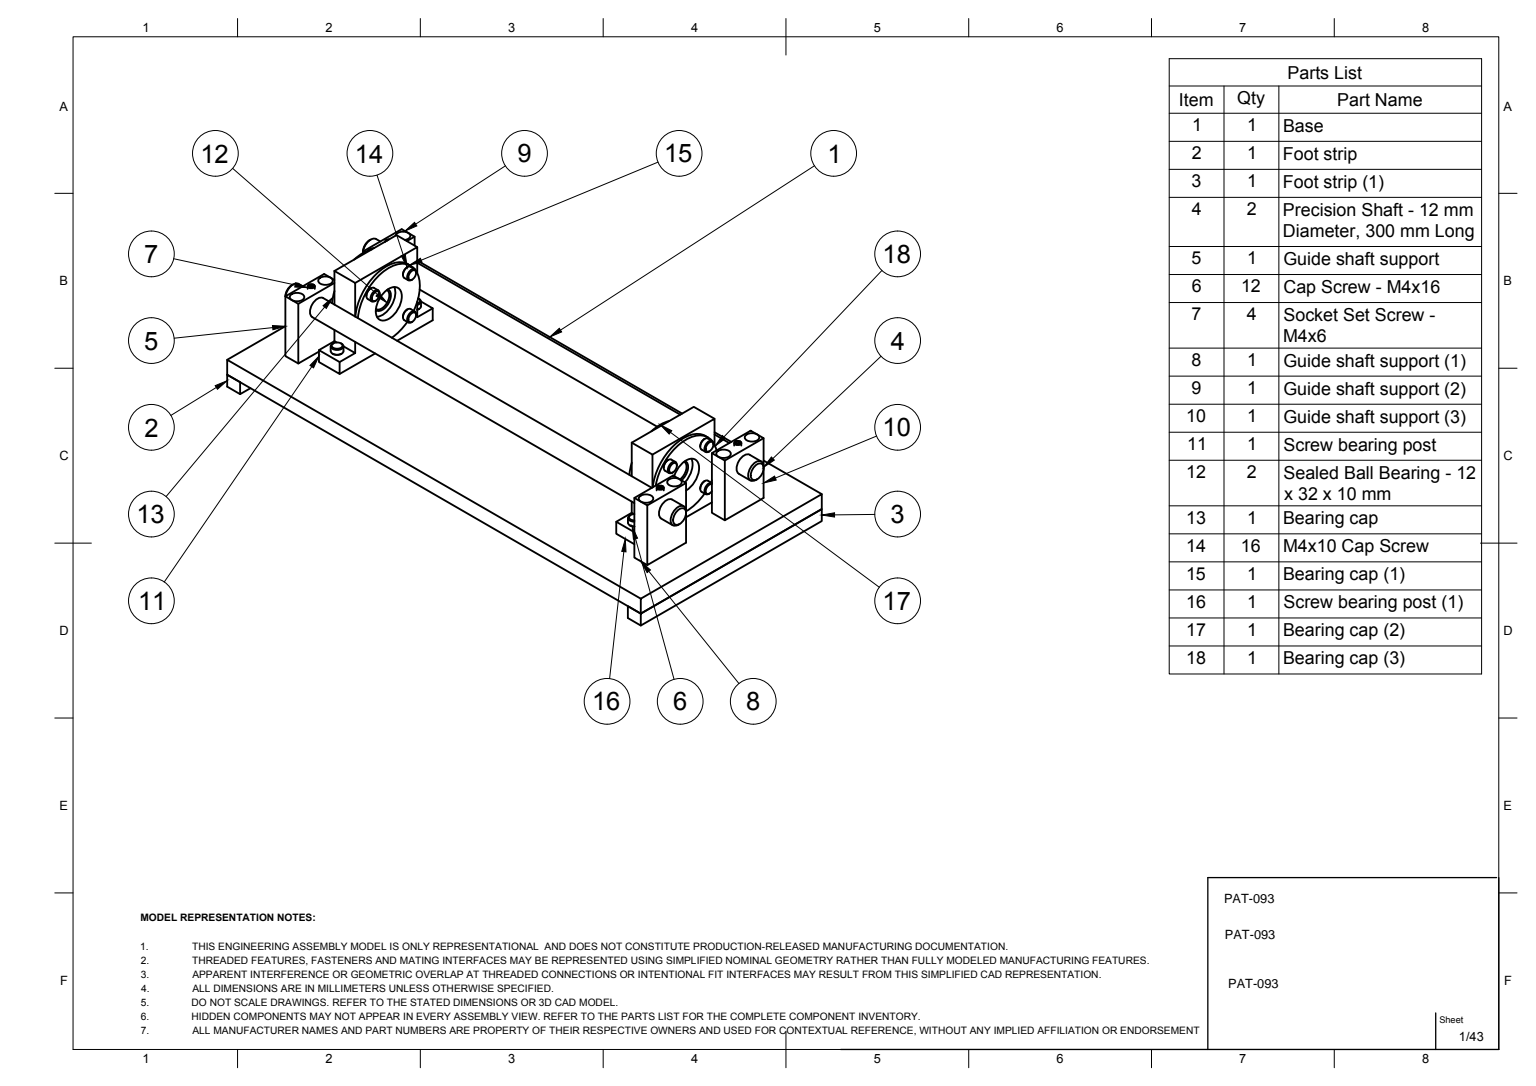
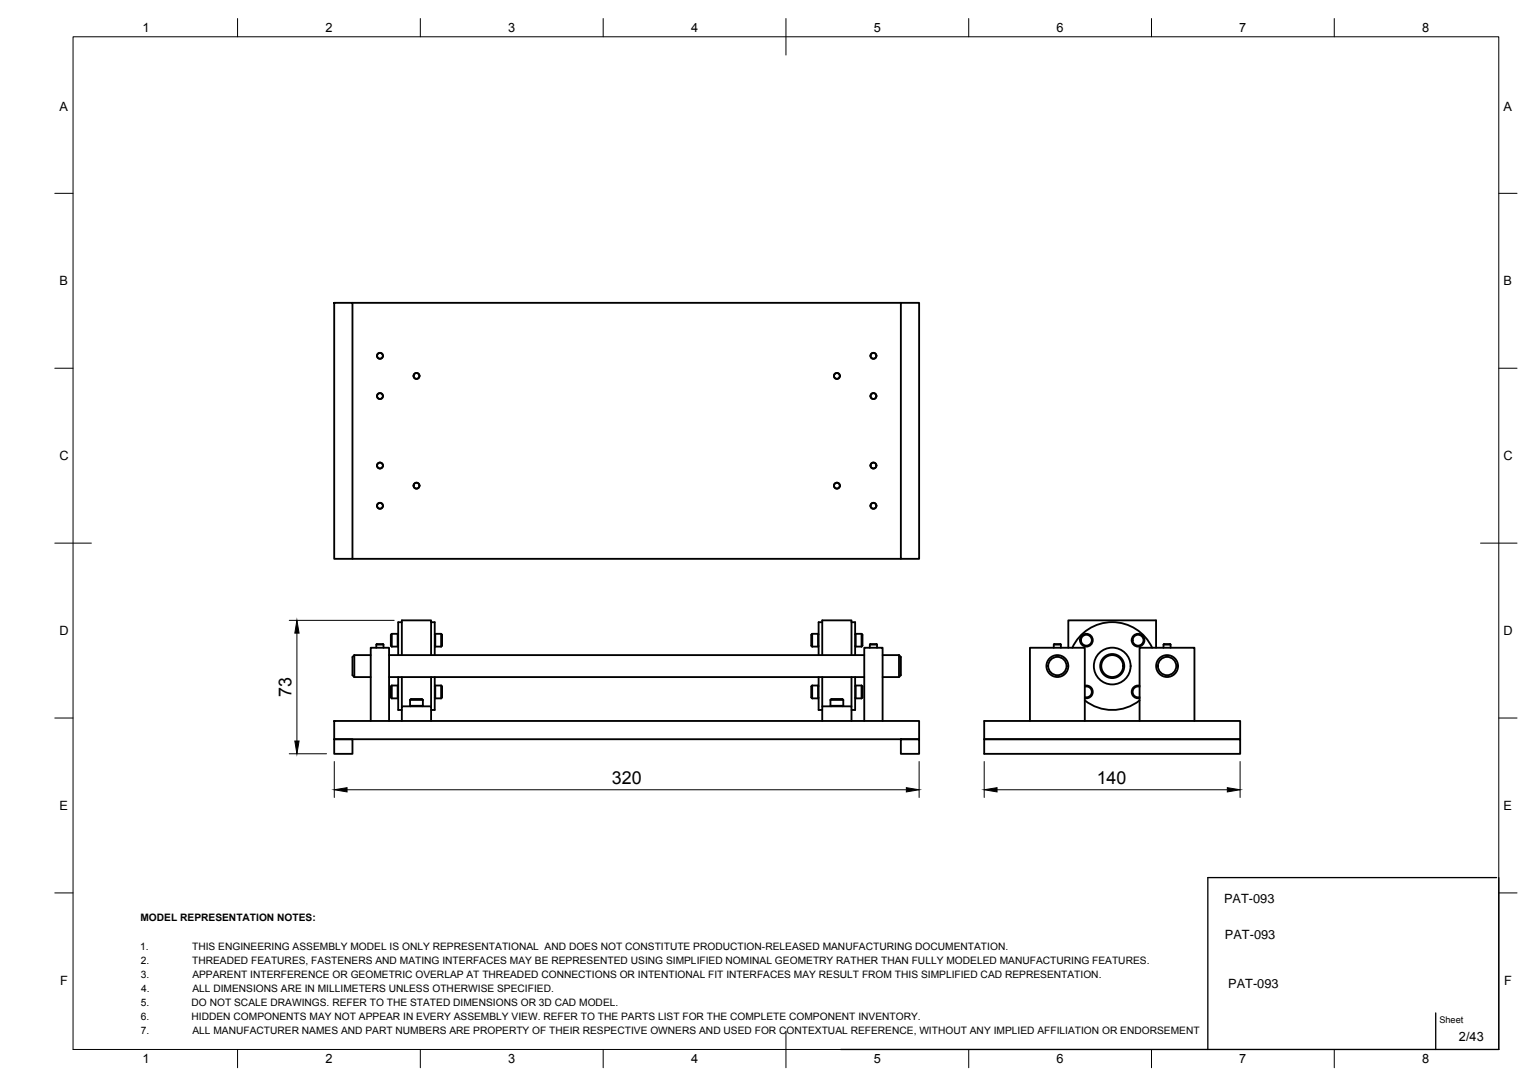
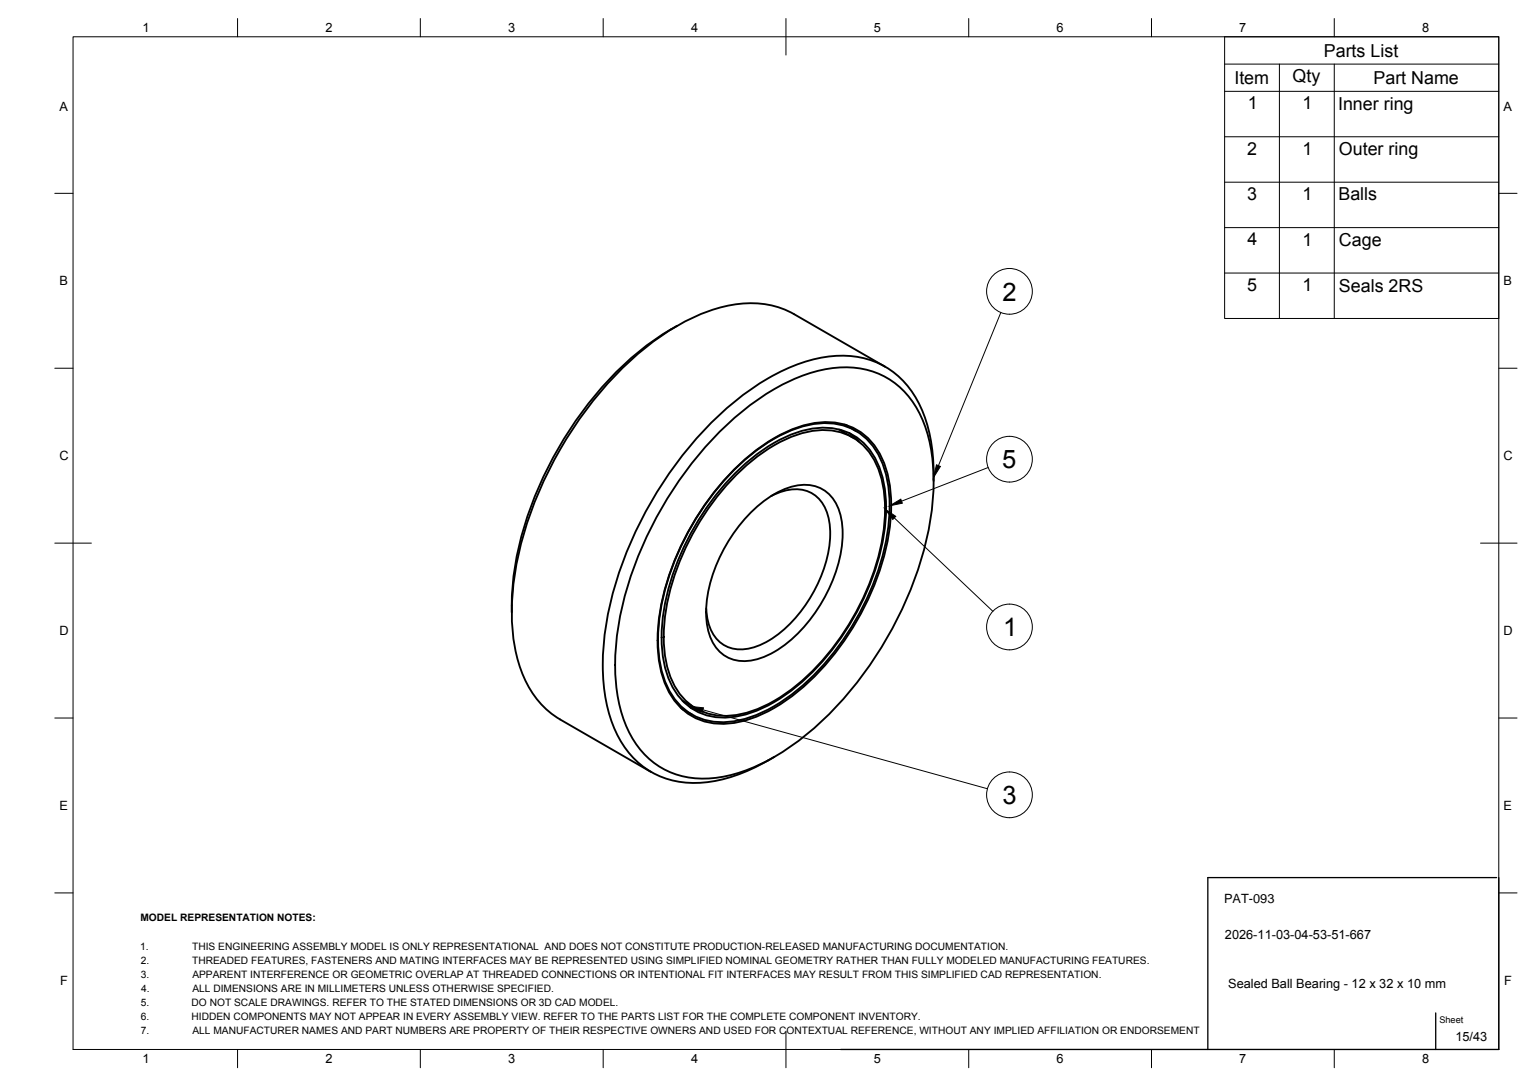
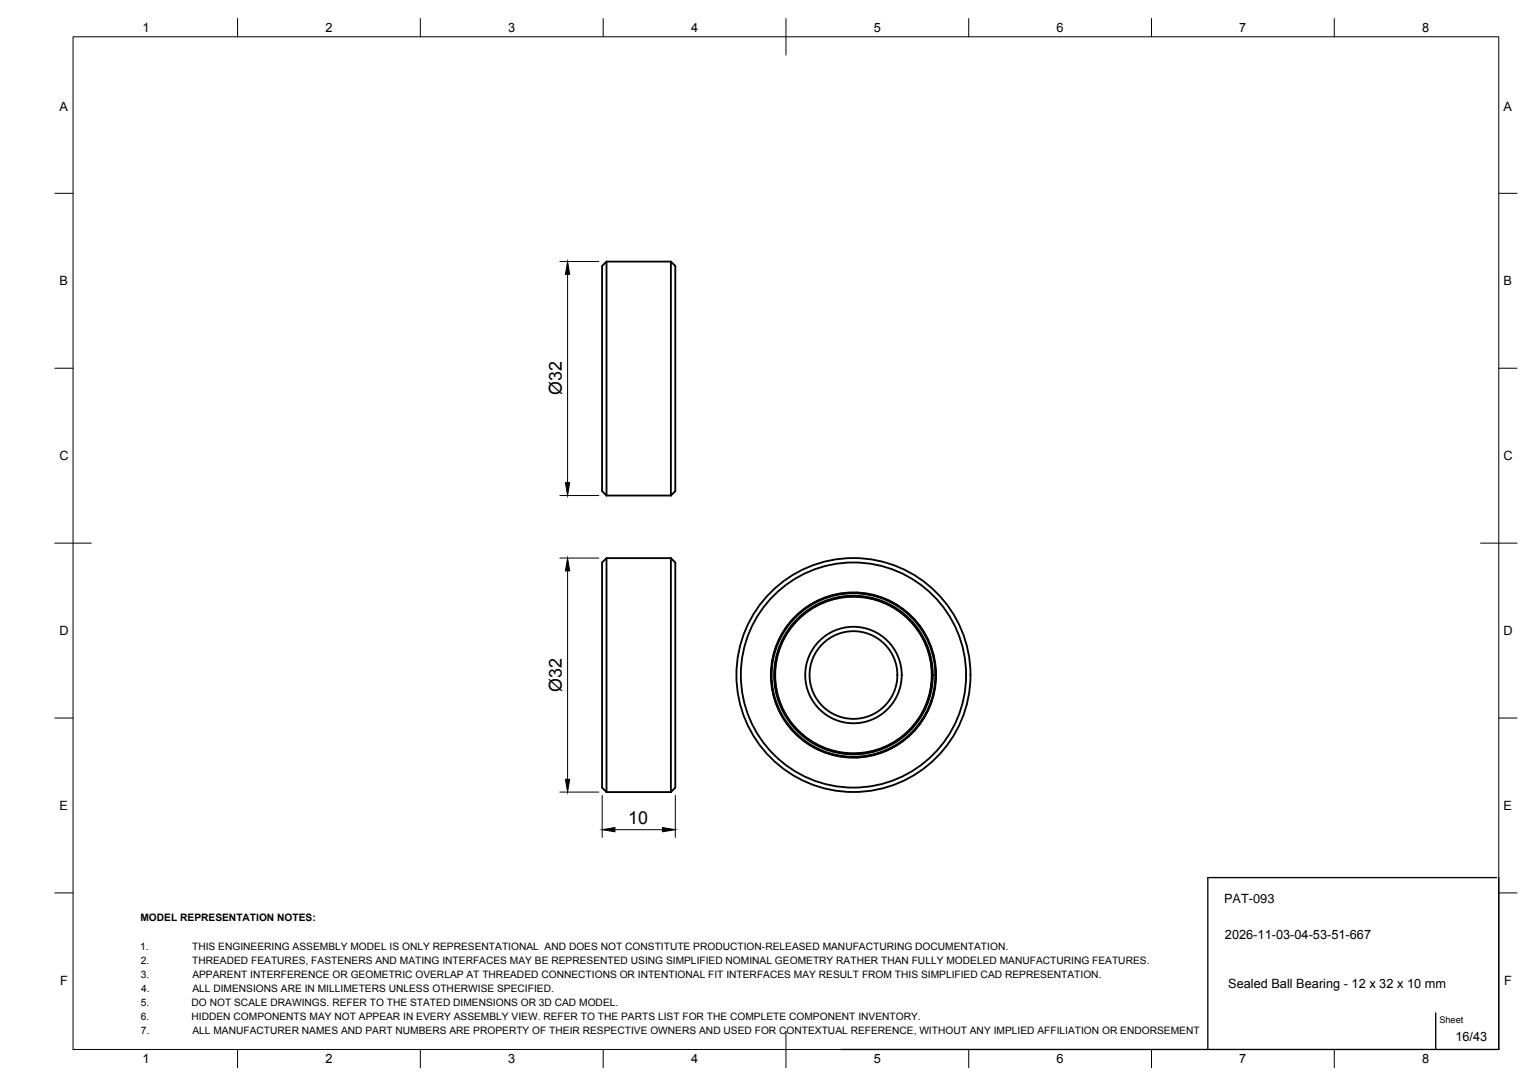
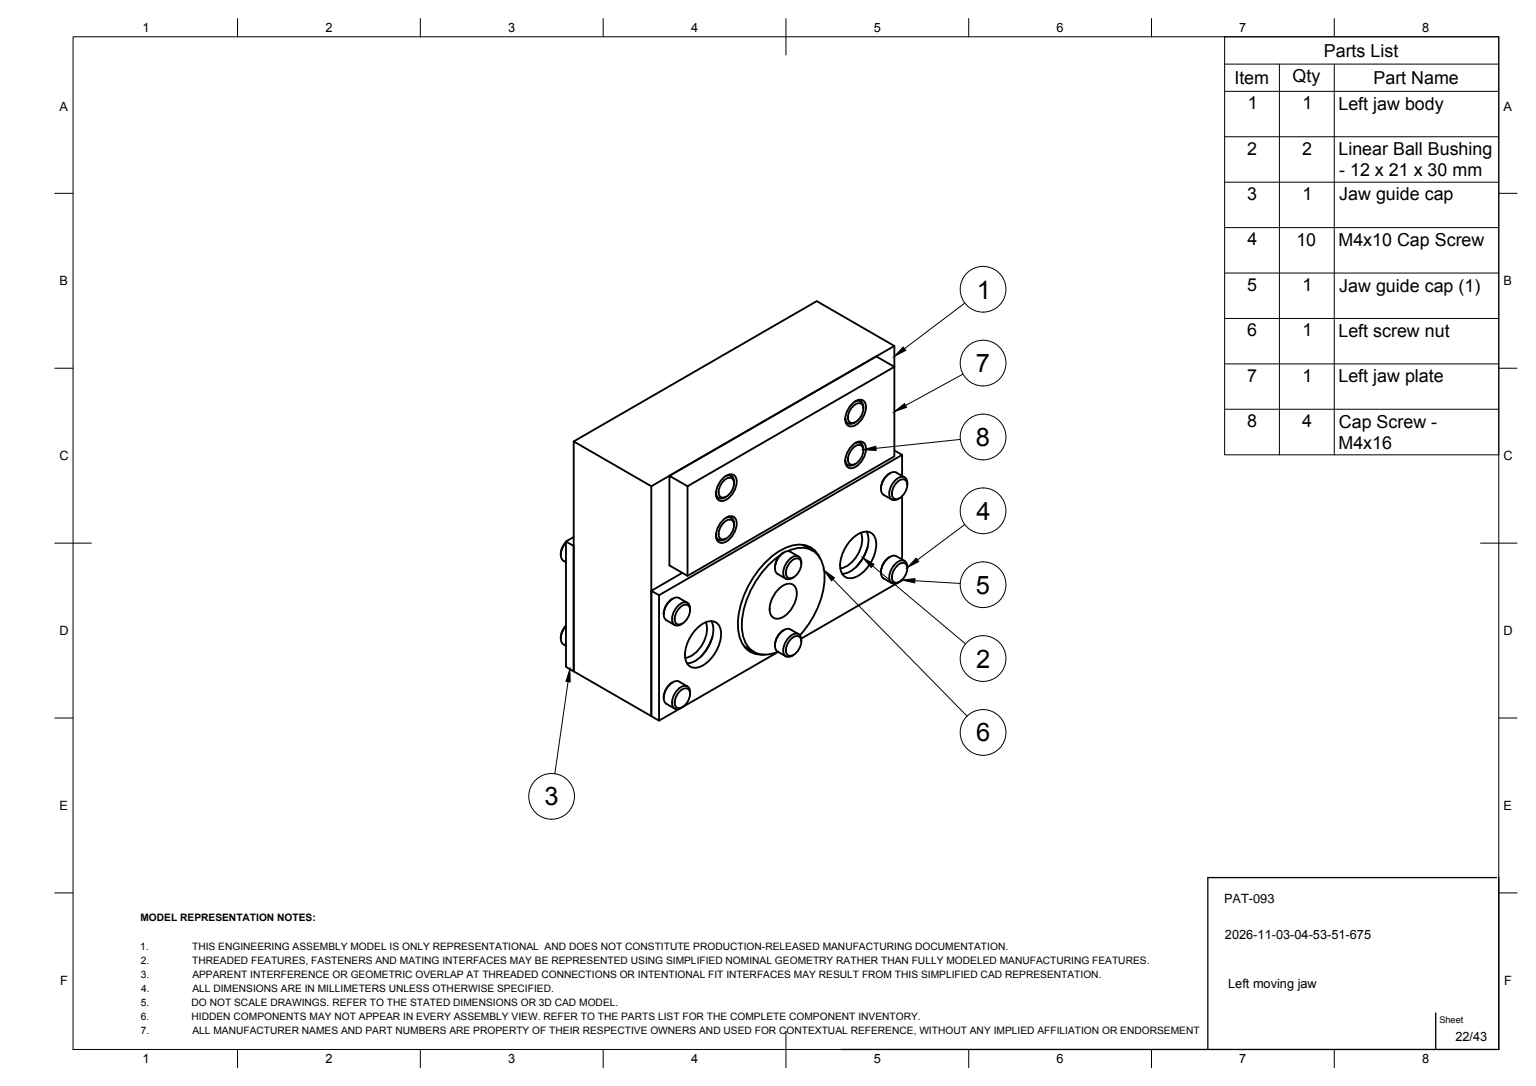
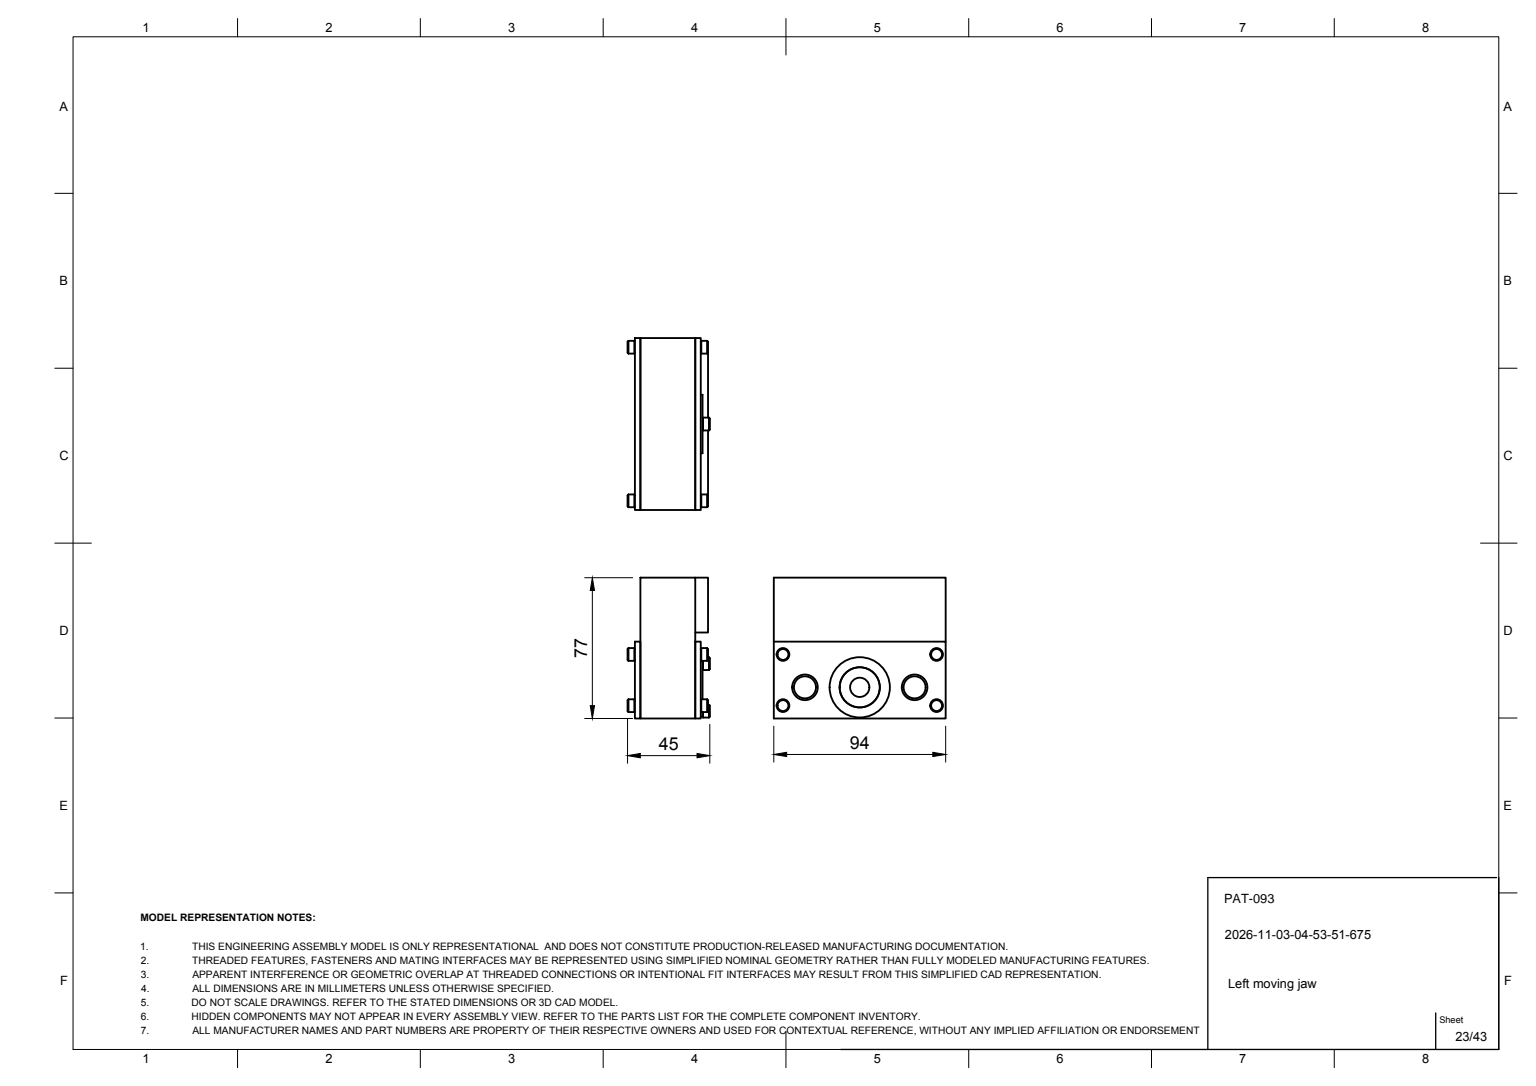
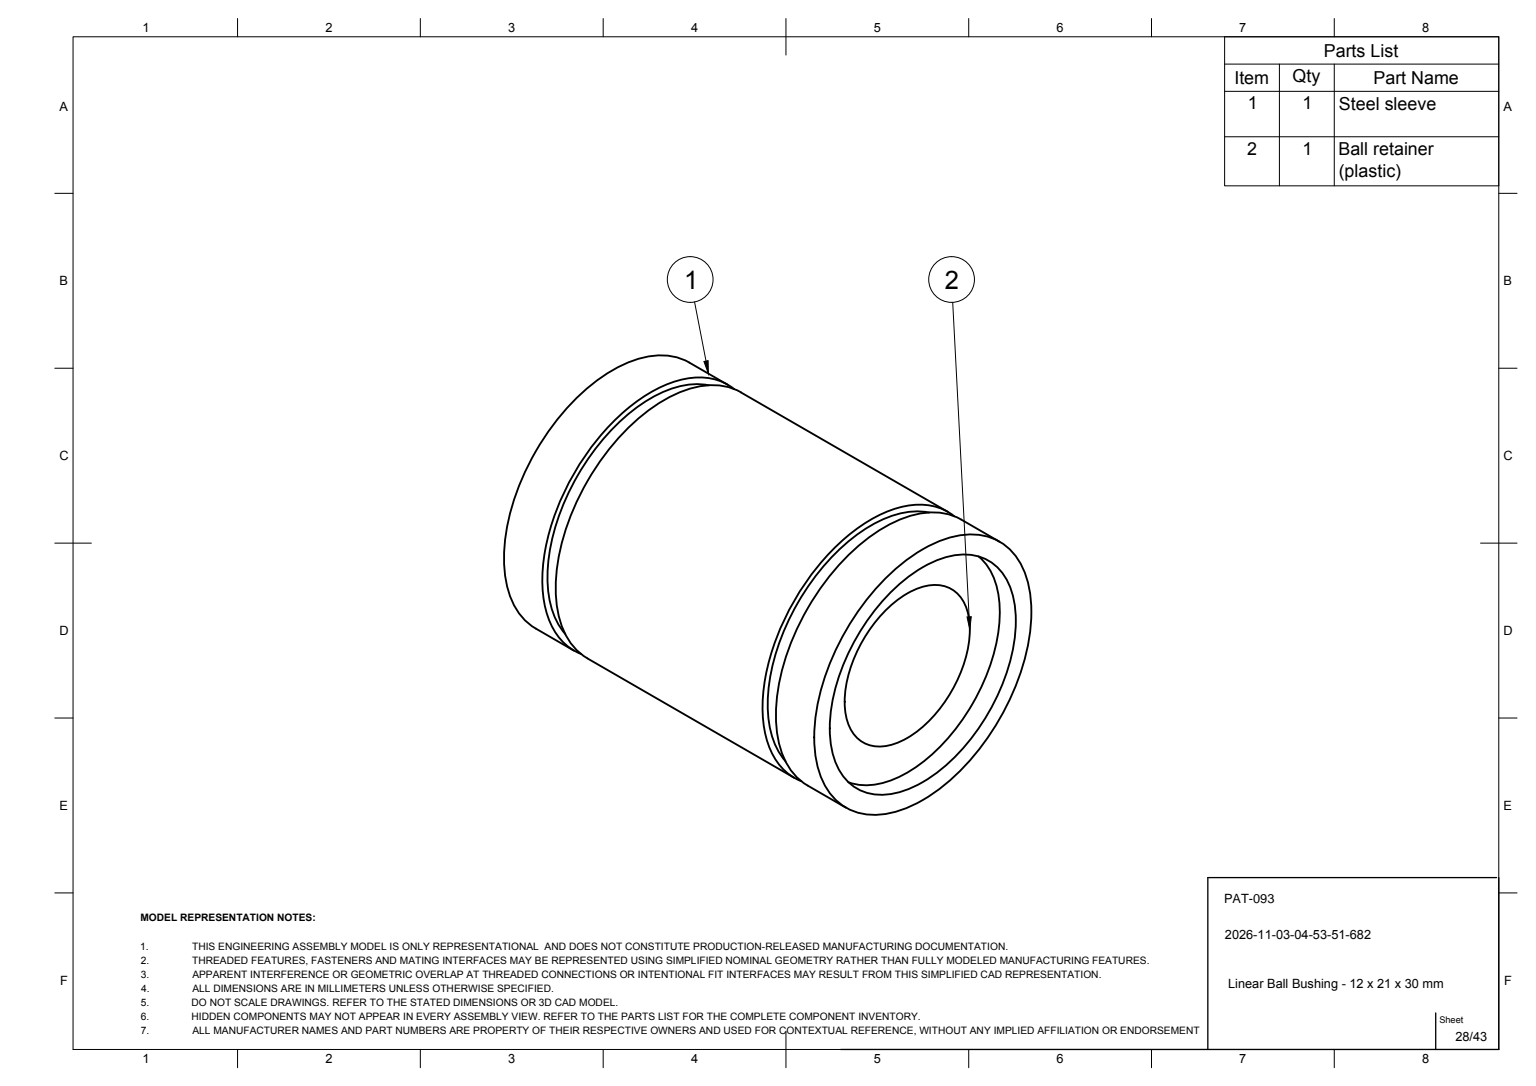
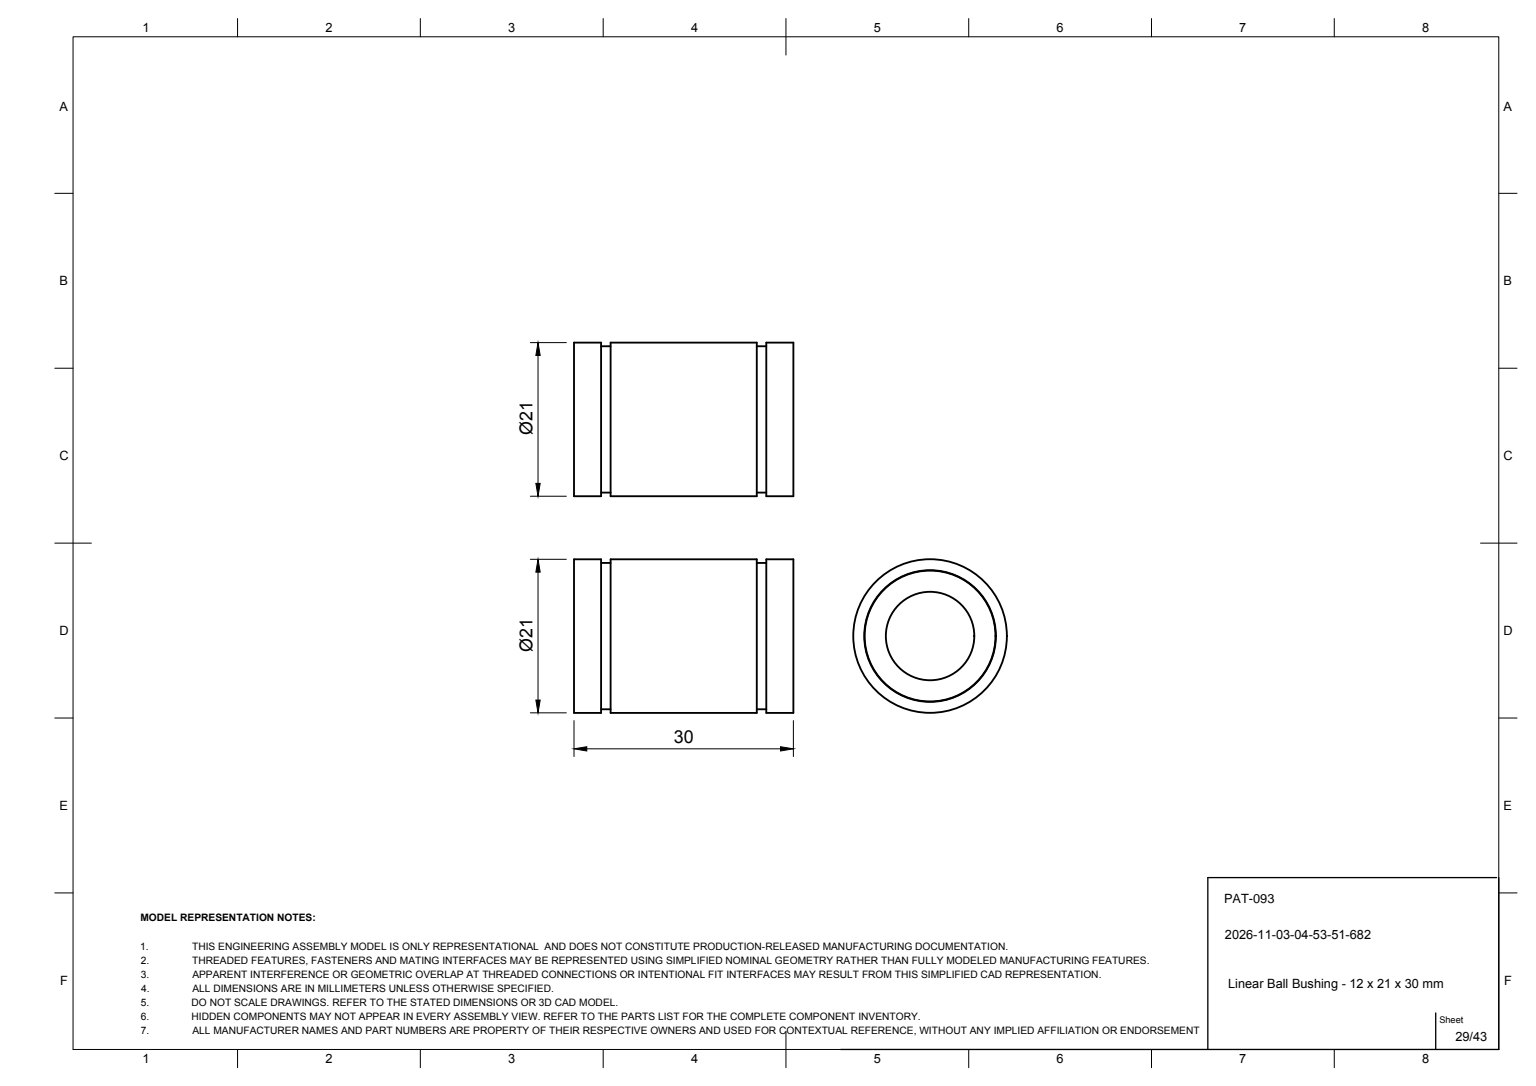
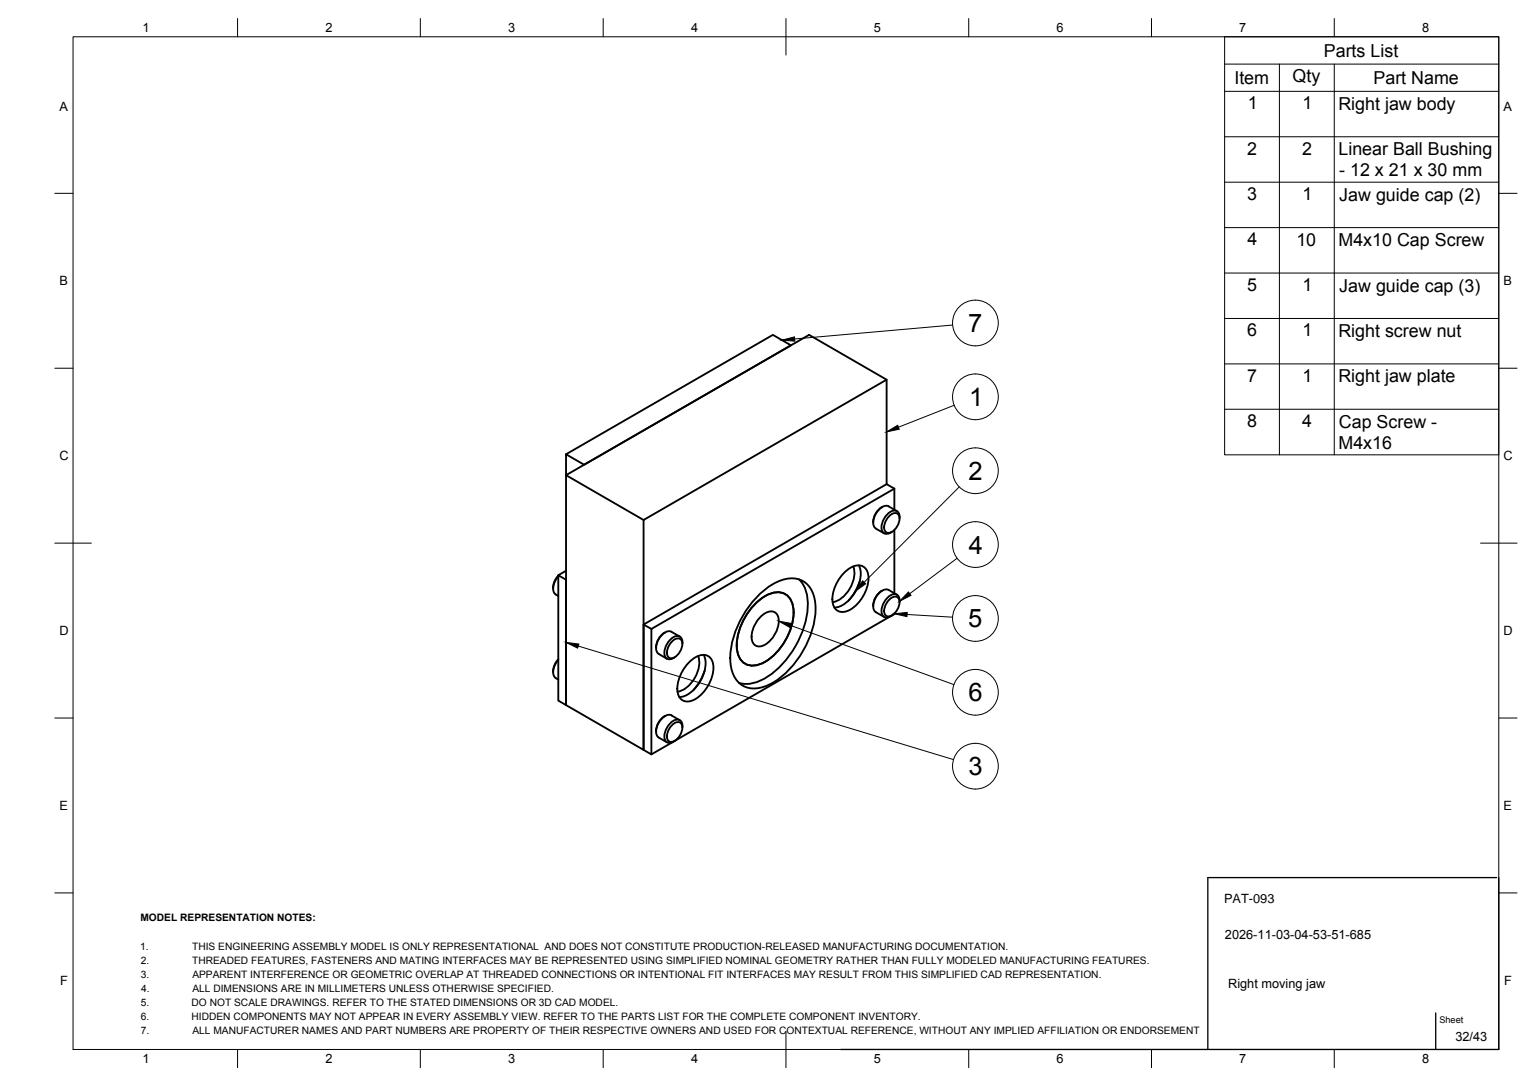
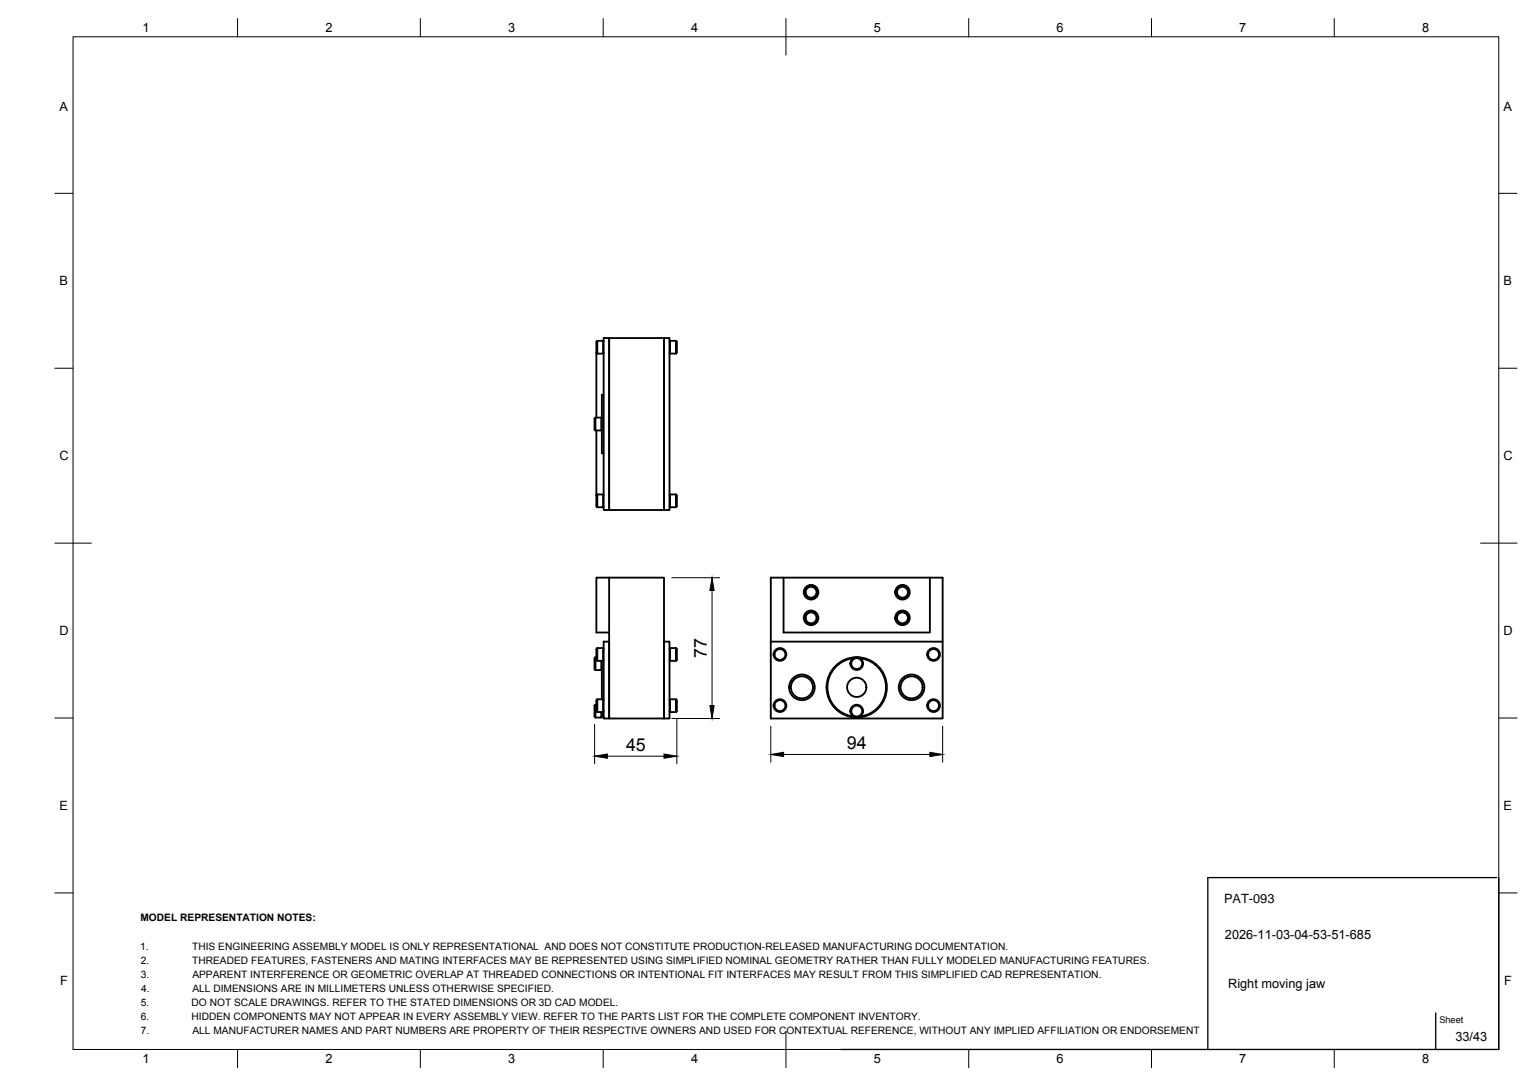
ISO-10303-21;
HEADER;
/* Generated by software containing ST-Developer
 * from STEP Tools, Inc. (www.steptools.com) 
 */

FILE_DESCRIPTION(
/* description */ ('Self-centering screw clamp'),
/* implementation_level */ '2;1');

FILE_NAME(
/* name */ 'PAT-093',
/* time_stamp */ '2026-10-28T03:25:31-07:00',
/* author */ (''),
/* organization */ (''),
/* preprocessor_version */ 'ST-DEVELOPER v20.2',
/* originating_system */ 'Autodesk Translation Framework v15.17.0.0',
/* authorisation */ '');

FILE_SCHEMA (('AUTOMOTIVE_DESIGN { 1 0 10303 214 3 1 1 }'));
ENDSEC;

DATA;
#10=MECHANICAL_DESIGN_GEOMETRIC_PRESENTATION_REPRESENTATION('',(#624,#625,
#626,#627,#628,#629,#630,#631,#632,#633,#634,#635,#636,#637,#638,#639,#640,
#641,#642,#643,#644,#645,#646,#647,#648,#649,#650,#651,#652,#653,#654,#655,
#656,#657,#658,#659,#660,#661,#662,#663,#664,#665,#666,#667,#668,#669,#670,
#671),#16799);
#11=ORIENTED_CLOSED_SHELL('',*,#9113,.F.);
#12=ORIENTED_CLOSED_SHELL('',*,#9123,.F.);
#13=BREP_WITH_VOIDS('Body1',#9114,(#11));
#14=BREP_WITH_VOIDS('Body1',#9122,(#12));
#15=ITEM_DEFINED_TRANSFORMATION($,$,#9955,#10077);
#16=ITEM_DEFINED_TRANSFORMATION($,$,#9975,#10078);
#17=ITEM_DEFINED_TRANSFORMATION($,$,#9995,#10079);
#18=ITEM_DEFINED_TRANSFORMATION($,$,#10010,#10080);
#19=ITEM_DEFINED_TRANSFORMATION($,$,#10060,#10081);
#20=ITEM_DEFINED_TRANSFORMATION($,$,#10429,#10478);
#21=ITEM_DEFINED_TRANSFORMATION($,$,#10461,#10479);
#22=ITEM_DEFINED_TRANSFORMATION($,$,#10083,#10629);
#23=ITEM_DEFINED_TRANSFORMATION($,$,#10135,#10630);
#24=ITEM_DEFINED_TRANSFORMATION($,$,#10163,#10631);
#25=ITEM_DEFINED_TRANSFORMATION($,$,#10191,#10632);
#26=ITEM_DEFINED_TRANSFORMATION($,$,#10220,#10633);
#27=ITEM_DEFINED_TRANSFORMATION($,$,#10428,#10634);
#28=ITEM_DEFINED_TRANSFORMATION($,$,#10428,#10635);
#29=ITEM_DEFINED_TRANSFORMATION($,$,#10480,#10636);
#30=ITEM_DEFINED_TRANSFORMATION($,$,#10480,#10637);
#31=ITEM_DEFINED_TRANSFORMATION($,$,#10480,#10638);
#32=ITEM_DEFINED_TRANSFORMATION($,$,#10480,#10639);
#33=ITEM_DEFINED_TRANSFORMATION($,$,#10480,#10640);
#34=ITEM_DEFINED_TRANSFORMATION($,$,#10480,#10641);
#35=ITEM_DEFINED_TRANSFORMATION($,$,#10480,#10642);
#36=ITEM_DEFINED_TRANSFORMATION($,$,#10480,#10643);
#37=ITEM_DEFINED_TRANSFORMATION($,$,#10480,#10644);
#38=ITEM_DEFINED_TRANSFORMATION($,$,#10480,#10645);
#39=ITEM_DEFINED_TRANSFORMATION($,$,#10603,#10646);
#40=ITEM_DEFINED_TRANSFORMATION($,$,#10603,#10647);
#41=ITEM_DEFINED_TRANSFORMATION($,$,#10603,#10648);
#42=ITEM_DEFINED_TRANSFORMATION($,$,#10603,#10649);
#43=ITEM_DEFINED_TRANSFORMATION($,$,#10256,#10650);
#44=ITEM_DEFINED_TRANSFORMATION($,$,#10308,#10651);
#45=ITEM_DEFINED_TRANSFORMATION($,$,#10336,#10652);
#46=ITEM_DEFINED_TRANSFORMATION($,$,#10364,#10653);
#47=ITEM_DEFINED_TRANSFORMATION($,$,#10393,#10654);
#48=ITEM_DEFINED_TRANSFORMATION($,$,#10428,#10655);
#49=ITEM_DEFINED_TRANSFORMATION($,$,#10428,#10656);
#50=ITEM_DEFINED_TRANSFORMATION($,$,#10480,#10657);
#51=ITEM_DEFINED_TRANSFORMATION($,$,#10480,#10658);
#52=ITEM_DEFINED_TRANSFORMATION($,$,#10480,#10659);
#53=ITEM_DEFINED_TRANSFORMATION($,$,#10480,#10660);
#54=ITEM_DEFINED_TRANSFORMATION($,$,#10480,#10661);
#55=ITEM_DEFINED_TRANSFORMATION($,$,#10480,#10662);
#56=ITEM_DEFINED_TRANSFORMATION($,$,#10480,#10663);
#57=ITEM_DEFINED_TRANSFORMATION($,$,#10480,#10664);
#58=ITEM_DEFINED_TRANSFORMATION($,$,#10480,#10665);
#59=ITEM_DEFINED_TRANSFORMATION($,$,#10480,#10666);
#60=ITEM_DEFINED_TRANSFORMATION($,$,#10603,#10667);
#61=ITEM_DEFINED_TRANSFORMATION($,$,#10603,#10668);
#62=ITEM_DEFINED_TRANSFORMATION($,$,#10603,#10669);
#63=ITEM_DEFINED_TRANSFORMATION($,$,#10603,#10670);
#64=ITEM_DEFINED_TRANSFORMATION($,$,#9579,#10688);
#65=ITEM_DEFINED_TRANSFORMATION($,$,#9622,#10689);
#66=ITEM_DEFINED_TRANSFORMATION($,$,#9629,#10690);
#67=ITEM_DEFINED_TRANSFORMATION($,$,#9636,#10691);
#68=ITEM_DEFINED_TRANSFORMATION($,$,#9672,#10692);
#69=ITEM_DEFINED_TRANSFORMATION($,$,#9708,#10693);
#70=ITEM_DEFINED_TRANSFORMATION($,$,#9744,#10694);
#71=ITEM_DEFINED_TRANSFORMATION($,$,#9780,#10695);
#72=ITEM_DEFINED_TRANSFORMATION($,$,#9812,#10696);
#73=ITEM_DEFINED_TRANSFORMATION($,$,#9837,#10697);
#74=ITEM_DEFINED_TRANSFORMATION($,$,#9862,#10698);
#75=ITEM_DEFINED_TRANSFORMATION($,$,#9894,#10699);
#76=ITEM_DEFINED_TRANSFORMATION($,$,#9919,#10700);
#77=ITEM_DEFINED_TRANSFORMATION($,$,#9944,#10701);
#78=ITEM_DEFINED_TRANSFORMATION($,$,#10603,#10702);
#79=ITEM_DEFINED_TRANSFORMATION($,$,#10603,#10703);
#80=ITEM_DEFINED_TRANSFORMATION($,$,#10671,#10704);
#81=ITEM_DEFINED_TRANSFORMATION($,$,#10603,#10705);
#82=ITEM_DEFINED_TRANSFORMATION($,$,#10603,#10706);
#83=ITEM_DEFINED_TRANSFORMATION($,$,#10671,#10707);
#84=ITEM_DEFINED_TRANSFORMATION($,$,#9944,#10708);
#85=ITEM_DEFINED_TRANSFORMATION($,$,#10603,#10709);
#86=ITEM_DEFINED_TRANSFORMATION($,$,#10603,#10710);
#87=ITEM_DEFINED_TRANSFORMATION($,$,#10671,#10711);
#88=ITEM_DEFINED_TRANSFORMATION($,$,#10603,#10712);
#89=ITEM_DEFINED_TRANSFORMATION($,$,#10603,#10713);
#90=ITEM_DEFINED_TRANSFORMATION($,$,#10671,#10714);
#91=ITEM_DEFINED_TRANSFORMATION($,$,#10603,#10715);
#92=ITEM_DEFINED_TRANSFORMATION($,$,#10603,#10716);
#93=ITEM_DEFINED_TRANSFORMATION($,$,#9954,#10717);
#94=ITEM_DEFINED_TRANSFORMATION($,$,#10480,#10718);
#95=ITEM_DEFINED_TRANSFORMATION($,$,#10480,#10719);
#96=ITEM_DEFINED_TRANSFORMATION($,$,#10480,#10720);
#97=ITEM_DEFINED_TRANSFORMATION($,$,#10480,#10721);
#98=ITEM_DEFINED_TRANSFORMATION($,$,#10480,#10722);
#99=ITEM_DEFINED_TRANSFORMATION($,$,#10480,#10723);
#100=ITEM_DEFINED_TRANSFORMATION($,$,#10480,#10724);
#101=ITEM_DEFINED_TRANSFORMATION($,$,#10480,#10725);
#102=ITEM_DEFINED_TRANSFORMATION($,$,#10603,#10726);
#103=ITEM_DEFINED_TRANSFORMATION($,$,#10603,#10727);
#104=ITEM_DEFINED_TRANSFORMATION($,$,#9954,#10728);
#105=ITEM_DEFINED_TRANSFORMATION($,$,#10480,#10729);
#106=ITEM_DEFINED_TRANSFORMATION($,$,#10480,#10730);
#107=ITEM_DEFINED_TRANSFORMATION($,$,#10480,#10731);
#108=ITEM_DEFINED_TRANSFORMATION($,$,#10480,#10732);
#109=ITEM_DEFINED_TRANSFORMATION($,$,#10480,#10733);
#110=ITEM_DEFINED_TRANSFORMATION($,$,#10480,#10734);
#111=ITEM_DEFINED_TRANSFORMATION($,$,#10480,#10735);
#112=ITEM_DEFINED_TRANSFORMATION($,$,#10480,#10736);
#113=ITEM_DEFINED_TRANSFORMATION($,$,#10505,#10737);
#114=ITEM_DEFINED_TRANSFORMATION($,$,#10535,#10738);
#115=ITEM_DEFINED_TRANSFORMATION($,$,#10544,#10739);
#116=ITEM_DEFINED_TRANSFORMATION($,$,#10553,#10740);
#117=ITEM_DEFINED_TRANSFORMATION($,$,#10571,#10741);
#118=ITEM_DEFINED_TRANSFORMATION($,$,#10580,#10742);
#119=ITEM_DEFINED_TRANSFORMATION($,$,#10589,#10743);
#120=ITEM_DEFINED_TRANSFORMATION($,$,#10671,#10744);
#121=ITEM_DEFINED_TRANSFORMATION($,$,#10603,#10745);
#122=ITEM_DEFINED_TRANSFORMATION($,$,#10603,#10746);
#123=ITEM_DEFINED_TRANSFORMATION($,$,#10671,#10747);
#124=ITEM_DEFINED_TRANSFORMATION($,$,#9578,#10748);
#125=ITEM_DEFINED_TRANSFORMATION($,$,#10082,#10749);
#126=ITEM_DEFINED_TRANSFORMATION($,$,#10255,#10750);
#127=ITEM_DEFINED_TRANSFORMATION($,$,#10504,#10751);
#128=(
REPRESENTATION_RELATIONSHIP($,$,#17030,#17029)
REPRESENTATION_RELATIONSHIP_WITH_TRANSFORMATION(#15)
SHAPE_REPRESENTATION_RELATIONSHIP()
);
#129=(
REPRESENTATION_RELATIONSHIP($,$,#17031,#17029)
REPRESENTATION_RELATIONSHIP_WITH_TRANSFORMATION(#16)
SHAPE_REPRESENTATION_RELATIONSHIP()
);
#130=(
REPRESENTATION_RELATIONSHIP($,$,#17032,#17029)
REPRESENTATION_RELATIONSHIP_WITH_TRANSFORMATION(#17)
SHAPE_REPRESENTATION_RELATIONSHIP()
);
#131=(
REPRESENTATION_RELATIONSHIP($,$,#17033,#17029)
REPRESENTATION_RELATIONSHIP_WITH_TRANSFORMATION(#18)
SHAPE_REPRESENTATION_RELATIONSHIP()
);
#132=(
REPRESENTATION_RELATIONSHIP($,$,#17034,#17029)
REPRESENTATION_RELATIONSHIP_WITH_TRANSFORMATION(#19)
SHAPE_REPRESENTATION_RELATIONSHIP()
);
#133=(
REPRESENTATION_RELATIONSHIP($,$,#17048,#17047)
REPRESENTATION_RELATIONSHIP_WITH_TRANSFORMATION(#20)
SHAPE_REPRESENTATION_RELATIONSHIP()
);
#134=(
REPRESENTATION_RELATIONSHIP($,$,#17049,#17047)
REPRESENTATION_RELATIONSHIP_WITH_TRANSFORMATION(#21)
SHAPE_REPRESENTATION_RELATIONSHIP()
);
#135=(
REPRESENTATION_RELATIONSHIP($,$,#17036,#17035)
REPRESENTATION_RELATIONSHIP_WITH_TRANSFORMATION(#22)
SHAPE_REPRESENTATION_RELATIONSHIP()
);
#136=(
REPRESENTATION_RELATIONSHIP($,$,#17037,#17035)
REPRESENTATION_RELATIONSHIP_WITH_TRANSFORMATION(#23)
SHAPE_REPRESENTATION_RELATIONSHIP()
);
#137=(
REPRESENTATION_RELATIONSHIP($,$,#17038,#17035)
REPRESENTATION_RELATIONSHIP_WITH_TRANSFORMATION(#24)
SHAPE_REPRESENTATION_RELATIONSHIP()
);
#138=(
REPRESENTATION_RELATIONSHIP($,$,#17039,#17035)
REPRESENTATION_RELATIONSHIP_WITH_TRANSFORMATION(#25)
SHAPE_REPRESENTATION_RELATIONSHIP()
);
#139=(
REPRESENTATION_RELATIONSHIP($,$,#17040,#17035)
REPRESENTATION_RELATIONSHIP_WITH_TRANSFORMATION(#26)
SHAPE_REPRESENTATION_RELATIONSHIP()
);
#140=(
REPRESENTATION_RELATIONSHIP($,$,#17047,#17035)
REPRESENTATION_RELATIONSHIP_WITH_TRANSFORMATION(#27)
SHAPE_REPRESENTATION_RELATIONSHIP()
);
#141=(
REPRESENTATION_RELATIONSHIP($,$,#17047,#17035)
REPRESENTATION_RELATIONSHIP_WITH_TRANSFORMATION(#28)
SHAPE_REPRESENTATION_RELATIONSHIP()
);
#142=(
REPRESENTATION_RELATIONSHIP($,$,#17050,#17035)
REPRESENTATION_RELATIONSHIP_WITH_TRANSFORMATION(#29)
SHAPE_REPRESENTATION_RELATIONSHIP()
);
#143=(
REPRESENTATION_RELATIONSHIP($,$,#17050,#17035)
REPRESENTATION_RELATIONSHIP_WITH_TRANSFORMATION(#30)
SHAPE_REPRESENTATION_RELATIONSHIP()
);
#144=(
REPRESENTATION_RELATIONSHIP($,$,#17050,#17035)
REPRESENTATION_RELATIONSHIP_WITH_TRANSFORMATION(#31)
SHAPE_REPRESENTATION_RELATIONSHIP()
);
#145=(
REPRESENTATION_RELATIONSHIP($,$,#17050,#17035)
REPRESENTATION_RELATIONSHIP_WITH_TRANSFORMATION(#32)
SHAPE_REPRESENTATION_RELATIONSHIP()
);
#146=(
REPRESENTATION_RELATIONSHIP($,$,#17050,#17035)
REPRESENTATION_RELATIONSHIP_WITH_TRANSFORMATION(#33)
SHAPE_REPRESENTATION_RELATIONSHIP()
);
#147=(
REPRESENTATION_RELATIONSHIP($,$,#17050,#17035)
REPRESENTATION_RELATIONSHIP_WITH_TRANSFORMATION(#34)
SHAPE_REPRESENTATION_RELATIONSHIP()
);
#148=(
REPRESENTATION_RELATIONSHIP($,$,#17050,#17035)
REPRESENTATION_RELATIONSHIP_WITH_TRANSFORMATION(#35)
SHAPE_REPRESENTATION_RELATIONSHIP()
);
#149=(
REPRESENTATION_RELATIONSHIP($,$,#17050,#17035)
REPRESENTATION_RELATIONSHIP_WITH_TRANSFORMATION(#36)
SHAPE_REPRESENTATION_RELATIONSHIP()
);
#150=(
REPRESENTATION_RELATIONSHIP($,$,#17050,#17035)
REPRESENTATION_RELATIONSHIP_WITH_TRANSFORMATION(#37)
SHAPE_REPRESENTATION_RELATIONSHIP()
);
#151=(
REPRESENTATION_RELATIONSHIP($,$,#17050,#17035)
REPRESENTATION_RELATIONSHIP_WITH_TRANSFORMATION(#38)
SHAPE_REPRESENTATION_RELATIONSHIP()
);
#152=(
REPRESENTATION_RELATIONSHIP($,$,#17059,#17035)
REPRESENTATION_RELATIONSHIP_WITH_TRANSFORMATION(#39)
SHAPE_REPRESENTATION_RELATIONSHIP()
);
#153=(
REPRESENTATION_RELATIONSHIP($,$,#17059,#17035)
REPRESENTATION_RELATIONSHIP_WITH_TRANSFORMATION(#40)
SHAPE_REPRESENTATION_RELATIONSHIP()
);
#154=(
REPRESENTATION_RELATIONSHIP($,$,#17059,#17035)
REPRESENTATION_RELATIONSHIP_WITH_TRANSFORMATION(#41)
SHAPE_REPRESENTATION_RELATIONSHIP()
);
#155=(
REPRESENTATION_RELATIONSHIP($,$,#17059,#17035)
REPRESENTATION_RELATIONSHIP_WITH_TRANSFORMATION(#42)
SHAPE_REPRESENTATION_RELATIONSHIP()
);
#156=(
REPRESENTATION_RELATIONSHIP($,$,#17042,#17041)
REPRESENTATION_RELATIONSHIP_WITH_TRANSFORMATION(#43)
SHAPE_REPRESENTATION_RELATIONSHIP()
);
#157=(
REPRESENTATION_RELATIONSHIP($,$,#17043,#17041)
REPRESENTATION_RELATIONSHIP_WITH_TRANSFORMATION(#44)
SHAPE_REPRESENTATION_RELATIONSHIP()
);
#158=(
REPRESENTATION_RELATIONSHIP($,$,#17044,#17041)
REPRESENTATION_RELATIONSHIP_WITH_TRANSFORMATION(#45)
SHAPE_REPRESENTATION_RELATIONSHIP()
);
#159=(
REPRESENTATION_RELATIONSHIP($,$,#17045,#17041)
REPRESENTATION_RELATIONSHIP_WITH_TRANSFORMATION(#46)
SHAPE_REPRESENTATION_RELATIONSHIP()
);
#160=(
REPRESENTATION_RELATIONSHIP($,$,#17046,#17041)
REPRESENTATION_RELATIONSHIP_WITH_TRANSFORMATION(#47)
SHAPE_REPRESENTATION_RELATIONSHIP()
);
#161=(
REPRESENTATION_RELATIONSHIP($,$,#17047,#17041)
REPRESENTATION_RELATIONSHIP_WITH_TRANSFORMATION(#48)
SHAPE_REPRESENTATION_RELATIONSHIP()
);
#162=(
REPRESENTATION_RELATIONSHIP($,$,#17047,#17041)
REPRESENTATION_RELATIONSHIP_WITH_TRANSFORMATION(#49)
SHAPE_REPRESENTATION_RELATIONSHIP()
);
#163=(
REPRESENTATION_RELATIONSHIP($,$,#17050,#17041)
REPRESENTATION_RELATIONSHIP_WITH_TRANSFORMATION(#50)
SHAPE_REPRESENTATION_RELATIONSHIP()
);
#164=(
REPRESENTATION_RELATIONSHIP($,$,#17050,#17041)
REPRESENTATION_RELATIONSHIP_WITH_TRANSFORMATION(#51)
SHAPE_REPRESENTATION_RELATIONSHIP()
);
#165=(
REPRESENTATION_RELATIONSHIP($,$,#17050,#17041)
REPRESENTATION_RELATIONSHIP_WITH_TRANSFORMATION(#52)
SHAPE_REPRESENTATION_RELATIONSHIP()
);
#166=(
REPRESENTATION_RELATIONSHIP($,$,#17050,#17041)
REPRESENTATION_RELATIONSHIP_WITH_TRANSFORMATION(#53)
SHAPE_REPRESENTATION_RELATIONSHIP()
);
#167=(
REPRESENTATION_RELATIONSHIP($,$,#17050,#17041)
REPRESENTATION_RELATIONSHIP_WITH_TRANSFORMATION(#54)
SHAPE_REPRESENTATION_RELATIONSHIP()
);
#168=(
REPRESENTATION_RELATIONSHIP($,$,#17050,#17041)
REPRESENTATION_RELATIONSHIP_WITH_TRANSFORMATION(#55)
SHAPE_REPRESENTATION_RELATIONSHIP()
);
#169=(
REPRESENTATION_RELATIONSHIP($,$,#17050,#17041)
REPRESENTATION_RELATIONSHIP_WITH_TRANSFORMATION(#56)
SHAPE_REPRESENTATION_RELATIONSHIP()
);
#170=(
REPRESENTATION_RELATIONSHIP($,$,#17050,#17041)
REPRESENTATION_RELATIONSHIP_WITH_TRANSFORMATION(#57)
SHAPE_REPRESENTATION_RELATIONSHIP()
);
#171=(
REPRESENTATION_RELATIONSHIP($,$,#17050,#17041)
REPRESENTATION_RELATIONSHIP_WITH_TRANSFORMATION(#58)
SHAPE_REPRESENTATION_RELATIONSHIP()
);
#172=(
REPRESENTATION_RELATIONSHIP($,$,#17050,#17041)
REPRESENTATION_RELATIONSHIP_WITH_TRANSFORMATION(#59)
SHAPE_REPRESENTATION_RELATIONSHIP()
);
#173=(
REPRESENTATION_RELATIONSHIP($,$,#17059,#17041)
REPRESENTATION_RELATIONSHIP_WITH_TRANSFORMATION(#60)
SHAPE_REPRESENTATION_RELATIONSHIP()
);
#174=(
REPRESENTATION_RELATIONSHIP($,$,#17059,#17041)
REPRESENTATION_RELATIONSHIP_WITH_TRANSFORMATION(#61)
SHAPE_REPRESENTATION_RELATIONSHIP()
);
#175=(
REPRESENTATION_RELATIONSHIP($,$,#17059,#17041)
REPRESENTATION_RELATIONSHIP_WITH_TRANSFORMATION(#62)
SHAPE_REPRESENTATION_RELATIONSHIP()
);
#176=(
REPRESENTATION_RELATIONSHIP($,$,#17059,#17041)
REPRESENTATION_RELATIONSHIP_WITH_TRANSFORMATION(#63)
SHAPE_REPRESENTATION_RELATIONSHIP()
);
#177=(
REPRESENTATION_RELATIONSHIP($,$,#17015,#17014)
REPRESENTATION_RELATIONSHIP_WITH_TRANSFORMATION(#64)
SHAPE_REPRESENTATION_RELATIONSHIP()
);
#178=(
REPRESENTATION_RELATIONSHIP($,$,#17016,#17014)
REPRESENTATION_RELATIONSHIP_WITH_TRANSFORMATION(#65)
SHAPE_REPRESENTATION_RELATIONSHIP()
);
#179=(
REPRESENTATION_RELATIONSHIP($,$,#17017,#17014)
REPRESENTATION_RELATIONSHIP_WITH_TRANSFORMATION(#66)
SHAPE_REPRESENTATION_RELATIONSHIP()
);
#180=(
REPRESENTATION_RELATIONSHIP($,$,#17018,#17014)
REPRESENTATION_RELATIONSHIP_WITH_TRANSFORMATION(#67)
SHAPE_REPRESENTATION_RELATIONSHIP()
);
#181=(
REPRESENTATION_RELATIONSHIP($,$,#17019,#17014)
REPRESENTATION_RELATIONSHIP_WITH_TRANSFORMATION(#68)
SHAPE_REPRESENTATION_RELATIONSHIP()
);
#182=(
REPRESENTATION_RELATIONSHIP($,$,#17020,#17014)
REPRESENTATION_RELATIONSHIP_WITH_TRANSFORMATION(#69)
SHAPE_REPRESENTATION_RELATIONSHIP()
);
#183=(
REPRESENTATION_RELATIONSHIP($,$,#17021,#17014)
REPRESENTATION_RELATIONSHIP_WITH_TRANSFORMATION(#70)
SHAPE_REPRESENTATION_RELATIONSHIP()
);
#184=(
REPRESENTATION_RELATIONSHIP($,$,#17022,#17014)
REPRESENTATION_RELATIONSHIP_WITH_TRANSFORMATION(#71)
SHAPE_REPRESENTATION_RELATIONSHIP()
);
#185=(
REPRESENTATION_RELATIONSHIP($,$,#17023,#17014)
REPRESENTATION_RELATIONSHIP_WITH_TRANSFORMATION(#72)
SHAPE_REPRESENTATION_RELATIONSHIP()
);
#186=(
REPRESENTATION_RELATIONSHIP($,$,#17024,#17014)
REPRESENTATION_RELATIONSHIP_WITH_TRANSFORMATION(#73)
SHAPE_REPRESENTATION_RELATIONSHIP()
);
#187=(
REPRESENTATION_RELATIONSHIP($,$,#17025,#17014)
REPRESENTATION_RELATIONSHIP_WITH_TRANSFORMATION(#74)
SHAPE_REPRESENTATION_RELATIONSHIP()
);
#188=(
REPRESENTATION_RELATIONSHIP($,$,#17026,#17014)
REPRESENTATION_RELATIONSHIP_WITH_TRANSFORMATION(#75)
SHAPE_REPRESENTATION_RELATIONSHIP()
);
#189=(
REPRESENTATION_RELATIONSHIP($,$,#17027,#17014)
REPRESENTATION_RELATIONSHIP_WITH_TRANSFORMATION(#76)
SHAPE_REPRESENTATION_RELATIONSHIP()
);
#190=(
REPRESENTATION_RELATIONSHIP($,$,#17028,#17014)
REPRESENTATION_RELATIONSHIP_WITH_TRANSFORMATION(#77)
SHAPE_REPRESENTATION_RELATIONSHIP()
);
#191=(
REPRESENTATION_RELATIONSHIP($,$,#17059,#17014)
REPRESENTATION_RELATIONSHIP_WITH_TRANSFORMATION(#78)
SHAPE_REPRESENTATION_RELATIONSHIP()
);
#192=(
REPRESENTATION_RELATIONSHIP($,$,#17059,#17014)
REPRESENTATION_RELATIONSHIP_WITH_TRANSFORMATION(#79)
SHAPE_REPRESENTATION_RELATIONSHIP()
);
#193=(
REPRESENTATION_RELATIONSHIP($,$,#17060,#17014)
REPRESENTATION_RELATIONSHIP_WITH_TRANSFORMATION(#80)
SHAPE_REPRESENTATION_RELATIONSHIP()
);
#194=(
REPRESENTATION_RELATIONSHIP($,$,#17059,#17014)
REPRESENTATION_RELATIONSHIP_WITH_TRANSFORMATION(#81)
SHAPE_REPRESENTATION_RELATIONSHIP()
);
#195=(
REPRESENTATION_RELATIONSHIP($,$,#17059,#17014)
REPRESENTATION_RELATIONSHIP_WITH_TRANSFORMATION(#82)
SHAPE_REPRESENTATION_RELATIONSHIP()
);
#196=(
REPRESENTATION_RELATIONSHIP($,$,#17060,#17014)
REPRESENTATION_RELATIONSHIP_WITH_TRANSFORMATION(#83)
SHAPE_REPRESENTATION_RELATIONSHIP()
);
#197=(
REPRESENTATION_RELATIONSHIP($,$,#17028,#17014)
REPRESENTATION_RELATIONSHIP_WITH_TRANSFORMATION(#84)
SHAPE_REPRESENTATION_RELATIONSHIP()
);
#198=(
REPRESENTATION_RELATIONSHIP($,$,#17059,#17014)
REPRESENTATION_RELATIONSHIP_WITH_TRANSFORMATION(#85)
SHAPE_REPRESENTATION_RELATIONSHIP()
);
#199=(
REPRESENTATION_RELATIONSHIP($,$,#17059,#17014)
REPRESENTATION_RELATIONSHIP_WITH_TRANSFORMATION(#86)
SHAPE_REPRESENTATION_RELATIONSHIP()
);
#200=(
REPRESENTATION_RELATIONSHIP($,$,#17060,#17014)
REPRESENTATION_RELATIONSHIP_WITH_TRANSFORMATION(#87)
SHAPE_REPRESENTATION_RELATIONSHIP()
);
#201=(
REPRESENTATION_RELATIONSHIP($,$,#17059,#17014)
REPRESENTATION_RELATIONSHIP_WITH_TRANSFORMATION(#88)
SHAPE_REPRESENTATION_RELATIONSHIP()
);
#202=(
REPRESENTATION_RELATIONSHIP($,$,#17059,#17014)
REPRESENTATION_RELATIONSHIP_WITH_TRANSFORMATION(#89)
SHAPE_REPRESENTATION_RELATIONSHIP()
);
#203=(
REPRESENTATION_RELATIONSHIP($,$,#17060,#17014)
REPRESENTATION_RELATIONSHIP_WITH_TRANSFORMATION(#90)
SHAPE_REPRESENTATION_RELATIONSHIP()
);
#204=(
REPRESENTATION_RELATIONSHIP($,$,#17059,#17014)
REPRESENTATION_RELATIONSHIP_WITH_TRANSFORMATION(#91)
SHAPE_REPRESENTATION_RELATIONSHIP()
);
#205=(
REPRESENTATION_RELATIONSHIP($,$,#17059,#17014)
REPRESENTATION_RELATIONSHIP_WITH_TRANSFORMATION(#92)
SHAPE_REPRESENTATION_RELATIONSHIP()
);
#206=(
REPRESENTATION_RELATIONSHIP($,$,#17029,#17014)
REPRESENTATION_RELATIONSHIP_WITH_TRANSFORMATION(#93)
SHAPE_REPRESENTATION_RELATIONSHIP()
);
#207=(
REPRESENTATION_RELATIONSHIP($,$,#17050,#17014)
REPRESENTATION_RELATIONSHIP_WITH_TRANSFORMATION(#94)
SHAPE_REPRESENTATION_RELATIONSHIP()
);
#208=(
REPRESENTATION_RELATIONSHIP($,$,#17050,#17014)
REPRESENTATION_RELATIONSHIP_WITH_TRANSFORMATION(#95)
SHAPE_REPRESENTATION_RELATIONSHIP()
);
#209=(
REPRESENTATION_RELATIONSHIP($,$,#17050,#17014)
REPRESENTATION_RELATIONSHIP_WITH_TRANSFORMATION(#96)
SHAPE_REPRESENTATION_RELATIONSHIP()
);
#210=(
REPRESENTATION_RELATIONSHIP($,$,#17050,#17014)
REPRESENTATION_RELATIONSHIP_WITH_TRANSFORMATION(#97)
SHAPE_REPRESENTATION_RELATIONSHIP()
);
#211=(
REPRESENTATION_RELATIONSHIP($,$,#17050,#17014)
REPRESENTATION_RELATIONSHIP_WITH_TRANSFORMATION(#98)
SHAPE_REPRESENTATION_RELATIONSHIP()
);
#212=(
REPRESENTATION_RELATIONSHIP($,$,#17050,#17014)
REPRESENTATION_RELATIONSHIP_WITH_TRANSFORMATION(#99)
SHAPE_REPRESENTATION_RELATIONSHIP()
);
#213=(
REPRESENTATION_RELATIONSHIP($,$,#17050,#17014)
REPRESENTATION_RELATIONSHIP_WITH_TRANSFORMATION(#100)
SHAPE_REPRESENTATION_RELATIONSHIP()
);
#214=(
REPRESENTATION_RELATIONSHIP($,$,#17050,#17014)
REPRESENTATION_RELATIONSHIP_WITH_TRANSFORMATION(#101)
SHAPE_REPRESENTATION_RELATIONSHIP()
);
#215=(
REPRESENTATION_RELATIONSHIP($,$,#17059,#17014)
REPRESENTATION_RELATIONSHIP_WITH_TRANSFORMATION(#102)
SHAPE_REPRESENTATION_RELATIONSHIP()
);
#216=(
REPRESENTATION_RELATIONSHIP($,$,#17059,#17014)
REPRESENTATION_RELATIONSHIP_WITH_TRANSFORMATION(#103)
SHAPE_REPRESENTATION_RELATIONSHIP()
);
#217=(
REPRESENTATION_RELATIONSHIP($,$,#17029,#17014)
REPRESENTATION_RELATIONSHIP_WITH_TRANSFORMATION(#104)
SHAPE_REPRESENTATION_RELATIONSHIP()
);
#218=(
REPRESENTATION_RELATIONSHIP($,$,#17050,#17014)
REPRESENTATION_RELATIONSHIP_WITH_TRANSFORMATION(#105)
SHAPE_REPRESENTATION_RELATIONSHIP()
);
#219=(
REPRESENTATION_RELATIONSHIP($,$,#17050,#17014)
REPRESENTATION_RELATIONSHIP_WITH_TRANSFORMATION(#106)
SHAPE_REPRESENTATION_RELATIONSHIP()
);
#220=(
REPRESENTATION_RELATIONSHIP($,$,#17050,#17014)
REPRESENTATION_RELATIONSHIP_WITH_TRANSFORMATION(#107)
SHAPE_REPRESENTATION_RELATIONSHIP()
);
#221=(
REPRESENTATION_RELATIONSHIP($,$,#17050,#17014)
REPRESENTATION_RELATIONSHIP_WITH_TRANSFORMATION(#108)
SHAPE_REPRESENTATION_RELATIONSHIP()
);
#222=(
REPRESENTATION_RELATIONSHIP($,$,#17050,#17014)
REPRESENTATION_RELATIONSHIP_WITH_TRANSFORMATION(#109)
SHAPE_REPRESENTATION_RELATIONSHIP()
);
#223=(
REPRESENTATION_RELATIONSHIP($,$,#17050,#17014)
REPRESENTATION_RELATIONSHIP_WITH_TRANSFORMATION(#110)
SHAPE_REPRESENTATION_RELATIONSHIP()
);
#224=(
REPRESENTATION_RELATIONSHIP($,$,#17050,#17014)
REPRESENTATION_RELATIONSHIP_WITH_TRANSFORMATION(#111)
SHAPE_REPRESENTATION_RELATIONSHIP()
);
#225=(
REPRESENTATION_RELATIONSHIP($,$,#17050,#17014)
REPRESENTATION_RELATIONSHIP_WITH_TRANSFORMATION(#112)
SHAPE_REPRESENTATION_RELATIONSHIP()
);
#226=(
REPRESENTATION_RELATIONSHIP($,$,#17052,#17051)
REPRESENTATION_RELATIONSHIP_WITH_TRANSFORMATION(#113)
SHAPE_REPRESENTATION_RELATIONSHIP()
);
#227=(
REPRESENTATION_RELATIONSHIP($,$,#17053,#17051)
REPRESENTATION_RELATIONSHIP_WITH_TRANSFORMATION(#114)
SHAPE_REPRESENTATION_RELATIONSHIP()
);
#228=(
REPRESENTATION_RELATIONSHIP($,$,#17054,#17051)
REPRESENTATION_RELATIONSHIP_WITH_TRANSFORMATION(#115)
SHAPE_REPRESENTATION_RELATIONSHIP()
);
#229=(
REPRESENTATION_RELATIONSHIP($,$,#17055,#17051)
REPRESENTATION_RELATIONSHIP_WITH_TRANSFORMATION(#116)
SHAPE_REPRESENTATION_RELATIONSHIP()
);
#230=(
REPRESENTATION_RELATIONSHIP($,$,#17056,#17051)
REPRESENTATION_RELATIONSHIP_WITH_TRANSFORMATION(#117)
SHAPE_REPRESENTATION_RELATIONSHIP()
);
#231=(
REPRESENTATION_RELATIONSHIP($,$,#17057,#17051)
REPRESENTATION_RELATIONSHIP_WITH_TRANSFORMATION(#118)
SHAPE_REPRESENTATION_RELATIONSHIP()
);
#232=(
REPRESENTATION_RELATIONSHIP($,$,#17058,#17051)
REPRESENTATION_RELATIONSHIP_WITH_TRANSFORMATION(#119)
SHAPE_REPRESENTATION_RELATIONSHIP()
);
#233=(
REPRESENTATION_RELATIONSHIP($,$,#17060,#17051)
REPRESENTATION_RELATIONSHIP_WITH_TRANSFORMATION(#120)
SHAPE_REPRESENTATION_RELATIONSHIP()
);
#234=(
REPRESENTATION_RELATIONSHIP($,$,#17059,#17051)
REPRESENTATION_RELATIONSHIP_WITH_TRANSFORMATION(#121)
SHAPE_REPRESENTATION_RELATIONSHIP()
);
#235=(
REPRESENTATION_RELATIONSHIP($,$,#17059,#17051)
REPRESENTATION_RELATIONSHIP_WITH_TRANSFORMATION(#122)
SHAPE_REPRESENTATION_RELATIONSHIP()
);
#236=(
REPRESENTATION_RELATIONSHIP($,$,#17060,#17051)
REPRESENTATION_RELATIONSHIP_WITH_TRANSFORMATION(#123)
SHAPE_REPRESENTATION_RELATIONSHIP()
);
#237=(
REPRESENTATION_RELATIONSHIP($,$,#17014,#17013)
REPRESENTATION_RELATIONSHIP_WITH_TRANSFORMATION(#124)
SHAPE_REPRESENTATION_RELATIONSHIP()
);
#238=(
REPRESENTATION_RELATIONSHIP($,$,#17035,#17013)
REPRESENTATION_RELATIONSHIP_WITH_TRANSFORMATION(#125)
SHAPE_REPRESENTATION_RELATIONSHIP()
);
#239=(
REPRESENTATION_RELATIONSHIP($,$,#17041,#17013)
REPRESENTATION_RELATIONSHIP_WITH_TRANSFORMATION(#126)
SHAPE_REPRESENTATION_RELATIONSHIP()
);
#240=(
REPRESENTATION_RELATIONSHIP($,$,#17051,#17013)
REPRESENTATION_RELATIONSHIP_WITH_TRANSFORMATION(#127)
SHAPE_REPRESENTATION_RELATIONSHIP()
);
#241=CONTEXT_DEPENDENT_SHAPE_REPRESENTATION(#128,#16874);
#242=CONTEXT_DEPENDENT_SHAPE_REPRESENTATION(#129,#16875);
#243=CONTEXT_DEPENDENT_SHAPE_REPRESENTATION(#130,#16876);
#244=CONTEXT_DEPENDENT_SHAPE_REPRESENTATION(#131,#16877);
#245=CONTEXT_DEPENDENT_SHAPE_REPRESENTATION(#132,#16878);
#246=CONTEXT_DEPENDENT_SHAPE_REPRESENTATION(#133,#16894);
#247=CONTEXT_DEPENDENT_SHAPE_REPRESENTATION(#134,#16895);
#248=CONTEXT_DEPENDENT_SHAPE_REPRESENTATION(#135,#16906);
#249=CONTEXT_DEPENDENT_SHAPE_REPRESENTATION(#136,#16907);
#250=CONTEXT_DEPENDENT_SHAPE_REPRESENTATION(#137,#16908);
#251=CONTEXT_DEPENDENT_SHAPE_REPRESENTATION(#138,#16909);
#252=CONTEXT_DEPENDENT_SHAPE_REPRESENTATION(#139,#16910);
#253=CONTEXT_DEPENDENT_SHAPE_REPRESENTATION(#140,#16911);
#254=CONTEXT_DEPENDENT_SHAPE_REPRESENTATION(#141,#16912);
#255=CONTEXT_DEPENDENT_SHAPE_REPRESENTATION(#142,#16913);
#256=CONTEXT_DEPENDENT_SHAPE_REPRESENTATION(#143,#16914);
#257=CONTEXT_DEPENDENT_SHAPE_REPRESENTATION(#144,#16915);
#258=CONTEXT_DEPENDENT_SHAPE_REPRESENTATION(#145,#16916);
#259=CONTEXT_DEPENDENT_SHAPE_REPRESENTATION(#146,#16917);
#260=CONTEXT_DEPENDENT_SHAPE_REPRESENTATION(#147,#16918);
#261=CONTEXT_DEPENDENT_SHAPE_REPRESENTATION(#148,#16919);
#262=CONTEXT_DEPENDENT_SHAPE_REPRESENTATION(#149,#16920);
#263=CONTEXT_DEPENDENT_SHAPE_REPRESENTATION(#150,#16921);
#264=CONTEXT_DEPENDENT_SHAPE_REPRESENTATION(#151,#16922);
#265=CONTEXT_DEPENDENT_SHAPE_REPRESENTATION(#152,#16923);
#266=CONTEXT_DEPENDENT_SHAPE_REPRESENTATION(#153,#16924);
#267=CONTEXT_DEPENDENT_SHAPE_REPRESENTATION(#154,#16925);
#268=CONTEXT_DEPENDENT_SHAPE_REPRESENTATION(#155,#16926);
#269=CONTEXT_DEPENDENT_SHAPE_REPRESENTATION(#156,#16927);
#270=CONTEXT_DEPENDENT_SHAPE_REPRESENTATION(#157,#16928);
#271=CONTEXT_DEPENDENT_SHAPE_REPRESENTATION(#158,#16929);
#272=CONTEXT_DEPENDENT_SHAPE_REPRESENTATION(#159,#16930);
#273=CONTEXT_DEPENDENT_SHAPE_REPRESENTATION(#160,#16931);
#274=CONTEXT_DEPENDENT_SHAPE_REPRESENTATION(#161,#16932);
#275=CONTEXT_DEPENDENT_SHAPE_REPRESENTATION(#162,#16933);
#276=CONTEXT_DEPENDENT_SHAPE_REPRESENTATION(#163,#16934);
#277=CONTEXT_DEPENDENT_SHAPE_REPRESENTATION(#164,#16935);
#278=CONTEXT_DEPENDENT_SHAPE_REPRESENTATION(#165,#16936);
#279=CONTEXT_DEPENDENT_SHAPE_REPRESENTATION(#166,#16937);
#280=CONTEXT_DEPENDENT_SHAPE_REPRESENTATION(#167,#16938);
#281=CONTEXT_DEPENDENT_SHAPE_REPRESENTATION(#168,#16939);
#282=CONTEXT_DEPENDENT_SHAPE_REPRESENTATION(#169,#16940);
#283=CONTEXT_DEPENDENT_SHAPE_REPRESENTATION(#170,#16941);
#284=CONTEXT_DEPENDENT_SHAPE_REPRESENTATION(#171,#16942);
#285=CONTEXT_DEPENDENT_SHAPE_REPRESENTATION(#172,#16943);
#286=CONTEXT_DEPENDENT_SHAPE_REPRESENTATION(#173,#16944);
#287=CONTEXT_DEPENDENT_SHAPE_REPRESENTATION(#174,#16945);
#288=CONTEXT_DEPENDENT_SHAPE_REPRESENTATION(#175,#16946);
#289=CONTEXT_DEPENDENT_SHAPE_REPRESENTATION(#176,#16947);
#290=CONTEXT_DEPENDENT_SHAPE_REPRESENTATION(#177,#16949);
#291=CONTEXT_DEPENDENT_SHAPE_REPRESENTATION(#178,#16950);
#292=CONTEXT_DEPENDENT_SHAPE_REPRESENTATION(#179,#16951);
#293=CONTEXT_DEPENDENT_SHAPE_REPRESENTATION(#180,#16952);
#294=CONTEXT_DEPENDENT_SHAPE_REPRESENTATION(#181,#16953);
#295=CONTEXT_DEPENDENT_SHAPE_REPRESENTATION(#182,#16954);
#296=CONTEXT_DEPENDENT_SHAPE_REPRESENTATION(#183,#16955);
#297=CONTEXT_DEPENDENT_SHAPE_REPRESENTATION(#184,#16956);
#298=CONTEXT_DEPENDENT_SHAPE_REPRESENTATION(#185,#16957);
#299=CONTEXT_DEPENDENT_SHAPE_REPRESENTATION(#186,#16958);
#300=CONTEXT_DEPENDENT_SHAPE_REPRESENTATION(#187,#16959);
#301=CONTEXT_DEPENDENT_SHAPE_REPRESENTATION(#188,#16960);
#302=CONTEXT_DEPENDENT_SHAPE_REPRESENTATION(#189,#16961);
#303=CONTEXT_DEPENDENT_SHAPE_REPRESENTATION(#190,#16962);
#304=CONTEXT_DEPENDENT_SHAPE_REPRESENTATION(#191,#16963);
#305=CONTEXT_DEPENDENT_SHAPE_REPRESENTATION(#192,#16964);
#306=CONTEXT_DEPENDENT_SHAPE_REPRESENTATION(#193,#16965);
#307=CONTEXT_DEPENDENT_SHAPE_REPRESENTATION(#194,#16966);
#308=CONTEXT_DEPENDENT_SHAPE_REPRESENTATION(#195,#16967);
#309=CONTEXT_DEPENDENT_SHAPE_REPRESENTATION(#196,#16968);
#310=CONTEXT_DEPENDENT_SHAPE_REPRESENTATION(#197,#16969);
#311=CONTEXT_DEPENDENT_SHAPE_REPRESENTATION(#198,#16970);
#312=CONTEXT_DEPENDENT_SHAPE_REPRESENTATION(#199,#16971);
#313=CONTEXT_DEPENDENT_SHAPE_REPRESENTATION(#200,#16972);
#314=CONTEXT_DEPENDENT_SHAPE_REPRESENTATION(#201,#16973);
#315=CONTEXT_DEPENDENT_SHAPE_REPRESENTATION(#202,#16974);
#316=CONTEXT_DEPENDENT_SHAPE_REPRESENTATION(#203,#16975);
#317=CONTEXT_DEPENDENT_SHAPE_REPRESENTATION(#204,#16976);
#318=CONTEXT_DEPENDENT_SHAPE_REPRESENTATION(#205,#16977);
#319=CONTEXT_DEPENDENT_SHAPE_REPRESENTATION(#206,#16978);
#320=CONTEXT_DEPENDENT_SHAPE_REPRESENTATION(#207,#16979);
#321=CONTEXT_DEPENDENT_SHAPE_REPRESENTATION(#208,#16980);
#322=CONTEXT_DEPENDENT_SHAPE_REPRESENTATION(#209,#16981);
#323=CONTEXT_DEPENDENT_SHAPE_REPRESENTATION(#210,#16982);
#324=CONTEXT_DEPENDENT_SHAPE_REPRESENTATION(#211,#16983);
#325=CONTEXT_DEPENDENT_SHAPE_REPRESENTATION(#212,#16984);
#326=CONTEXT_DEPENDENT_SHAPE_REPRESENTATION(#213,#16985);
#327=CONTEXT_DEPENDENT_SHAPE_REPRESENTATION(#214,#16986);
#328=CONTEXT_DEPENDENT_SHAPE_REPRESENTATION(#215,#16987);
#329=CONTEXT_DEPENDENT_SHAPE_REPRESENTATION(#216,#16988);
#330=CONTEXT_DEPENDENT_SHAPE_REPRESENTATION(#217,#16989);
#331=CONTEXT_DEPENDENT_SHAPE_REPRESENTATION(#218,#16990);
#332=CONTEXT_DEPENDENT_SHAPE_REPRESENTATION(#219,#16991);
#333=CONTEXT_DEPENDENT_SHAPE_REPRESENTATION(#220,#16992);
#334=CONTEXT_DEPENDENT_SHAPE_REPRESENTATION(#221,#16993);
#335=CONTEXT_DEPENDENT_SHAPE_REPRESENTATION(#222,#16994);
#336=CONTEXT_DEPENDENT_SHAPE_REPRESENTATION(#223,#16995);
#337=CONTEXT_DEPENDENT_SHAPE_REPRESENTATION(#224,#16996);
#338=CONTEXT_DEPENDENT_SHAPE_REPRESENTATION(#225,#16997);
#339=CONTEXT_DEPENDENT_SHAPE_REPRESENTATION(#226,#16998);
#340=CONTEXT_DEPENDENT_SHAPE_REPRESENTATION(#227,#16999);
#341=CONTEXT_DEPENDENT_SHAPE_REPRESENTATION(#228,#17000);
#342=CONTEXT_DEPENDENT_SHAPE_REPRESENTATION(#229,#17001);
#343=CONTEXT_DEPENDENT_SHAPE_REPRESENTATION(#230,#17002);
#344=CONTEXT_DEPENDENT_SHAPE_REPRESENTATION(#231,#17003);
#345=CONTEXT_DEPENDENT_SHAPE_REPRESENTATION(#232,#17004);
#346=CONTEXT_DEPENDENT_SHAPE_REPRESENTATION(#233,#17005);
#347=CONTEXT_DEPENDENT_SHAPE_REPRESENTATION(#234,#17006);
#348=CONTEXT_DEPENDENT_SHAPE_REPRESENTATION(#235,#17007);
#349=CONTEXT_DEPENDENT_SHAPE_REPRESENTATION(#236,#17008);
#350=CONTEXT_DEPENDENT_SHAPE_REPRESENTATION(#237,#17009);
#351=CONTEXT_DEPENDENT_SHAPE_REPRESENTATION(#238,#17010);
#352=CONTEXT_DEPENDENT_SHAPE_REPRESENTATION(#239,#17011);
#353=CONTEXT_DEPENDENT_SHAPE_REPRESENTATION(#240,#17012);
#354=NEXT_ASSEMBLY_USAGE_OCCURRENCE('Inner ring:1','Inner ring:1',
'Inner ring:1',#17078,#17079,'Inner ring:1');
#355=NEXT_ASSEMBLY_USAGE_OCCURRENCE('Outer ring:1','Outer ring:1',
'Outer ring:1',#17078,#17080,'Outer ring:1');
#356=NEXT_ASSEMBLY_USAGE_OCCURRENCE('Balls:1','Balls:1','Balls:1',#17078,
#17081,'Balls:1');
#357=NEXT_ASSEMBLY_USAGE_OCCURRENCE('Cage:1','Cage:1','Cage:1',#17078,#17082,
'Cage:1');
#358=NEXT_ASSEMBLY_USAGE_OCCURRENCE('Seals 2RS:1','Seals 2RS:1',
'Seals 2RS:1',#17078,#17083,'Seals 2RS:1');
#359=NEXT_ASSEMBLY_USAGE_OCCURRENCE('Steel sleeve:1','Steel sleeve:1',
'Steel sleeve:1',#17096,#17097,'Steel sleeve:1');
#360=NEXT_ASSEMBLY_USAGE_OCCURRENCE('Ball retainer (plastic):1',
'Ball retainer (plastic):1','Ball retainer (plastic):1',#17096,#17098,
'Ball retainer (plastic):1');
#361=NEXT_ASSEMBLY_USAGE_OCCURRENCE('Left jaw body:1','Left jaw body:1',
'Left jaw body:1',#17084,#17085,'Left jaw body:1');
#362=NEXT_ASSEMBLY_USAGE_OCCURRENCE('Jaw guide cap:1','Jaw guide cap:1',
'Jaw guide cap:1',#17084,#17086,'Jaw guide cap:1');
#363=NEXT_ASSEMBLY_USAGE_OCCURRENCE('Jaw guide cap (1):1',
'Jaw guide cap (1):1','Jaw guide cap (1):1',#17084,#17087,
'Jaw guide cap (1):1');
#364=NEXT_ASSEMBLY_USAGE_OCCURRENCE('Left screw nut:1',
'Left screw nut:1','Left screw nut:1',#17084,#17088,'Left screw nut:1');
#365=NEXT_ASSEMBLY_USAGE_OCCURRENCE('Left jaw plate:1',
'Left jaw plate:1','Left jaw plate:1',#17084,#17089,'Left jaw plate:1');
#366=NEXT_ASSEMBLY_USAGE_OCCURRENCE(
'Linear Ball Bushing - 12 x 21 x 30 mm:2',
'Linear Ball Bushing - 12 x 21 x 30 mm:2',
'Linear Ball Bushing - 12 x 21 x 30 mm:2',#17084,#17096,
'Linear Ball Bushing - 12 x 21 x 30 mm:2');
#367=NEXT_ASSEMBLY_USAGE_OCCURRENCE(
'Linear Ball Bushing - 12 x 21 x 30 mm:3',
'Linear Ball Bushing - 12 x 21 x 30 mm:3',
'Linear Ball Bushing - 12 x 21 x 30 mm:3',#17084,#17096,
'Linear Ball Bushing - 12 x 21 x 30 mm:3');
#368=NEXT_ASSEMBLY_USAGE_OCCURRENCE('M4x10 Cap Screw:18',
'M4x10 Cap Screw:18','M4x10 Cap Screw:18',#17084,#17099,
'M4x10 Cap Screw:18');
#369=NEXT_ASSEMBLY_USAGE_OCCURRENCE('M4x10 Cap Screw:19',
'M4x10 Cap Screw:19','M4x10 Cap Screw:19',#17084,#17099,
'M4x10 Cap Screw:19');
#370=NEXT_ASSEMBLY_USAGE_OCCURRENCE('M4x10 Cap Screw:20',
'M4x10 Cap Screw:20','M4x10 Cap Screw:20',#17084,#17099,
'M4x10 Cap Screw:20');
#371=NEXT_ASSEMBLY_USAGE_OCCURRENCE('M4x10 Cap Screw:21',
'M4x10 Cap Screw:21','M4x10 Cap Screw:21',#17084,#17099,
'M4x10 Cap Screw:21');
#372=NEXT_ASSEMBLY_USAGE_OCCURRENCE('M4x10 Cap Screw:22',
'M4x10 Cap Screw:22','M4x10 Cap Screw:22',#17084,#17099,
'M4x10 Cap Screw:22');
#373=NEXT_ASSEMBLY_USAGE_OCCURRENCE('M4x10 Cap Screw:23',
'M4x10 Cap Screw:23','M4x10 Cap Screw:23',#17084,#17099,
'M4x10 Cap Screw:23');
#374=NEXT_ASSEMBLY_USAGE_OCCURRENCE('M4x10 Cap Screw:24',
'M4x10 Cap Screw:24','M4x10 Cap Screw:24',#17084,#17099,
'M4x10 Cap Screw:24');
#375=NEXT_ASSEMBLY_USAGE_OCCURRENCE('M4x10 Cap Screw:25',
'M4x10 Cap Screw:25','M4x10 Cap Screw:25',#17084,#17099,
'M4x10 Cap Screw:25');
#376=NEXT_ASSEMBLY_USAGE_OCCURRENCE('M4x10 Cap Screw:26',
'M4x10 Cap Screw:26','M4x10 Cap Screw:26',#17084,#17099,
'M4x10 Cap Screw:26');
#377=NEXT_ASSEMBLY_USAGE_OCCURRENCE('M4x10 Cap Screw:27',
'M4x10 Cap Screw:27','M4x10 Cap Screw:27',#17084,#17099,
'M4x10 Cap Screw:27');
#378=NEXT_ASSEMBLY_USAGE_OCCURRENCE('Cap Screw - M4x16:14',
'Cap Screw - M4x16:14','Cap Screw - M4x16:14',#17084,#17108,
'Cap Screw - M4x16:14');
#379=NEXT_ASSEMBLY_USAGE_OCCURRENCE('Cap Screw - M4x16:15',
'Cap Screw - M4x16:15','Cap Screw - M4x16:15',#17084,#17108,
'Cap Screw - M4x16:15');
#380=NEXT_ASSEMBLY_USAGE_OCCURRENCE('Cap Screw - M4x16:16',
'Cap Screw - M4x16:16','Cap Screw - M4x16:16',#17084,#17108,
'Cap Screw - M4x16:16');
#381=NEXT_ASSEMBLY_USAGE_OCCURRENCE('Cap Screw - M4x16:17',
'Cap Screw - M4x16:17','Cap Screw - M4x16:17',#17084,#17108,
'Cap Screw - M4x16:17');
#382=NEXT_ASSEMBLY_USAGE_OCCURRENCE('Right jaw body:1',
'Right jaw body:1','Right jaw body:1',#17090,#17091,'Right jaw body:1');
#383=NEXT_ASSEMBLY_USAGE_OCCURRENCE('Jaw guide cap (2):1',
'Jaw guide cap (2):1','Jaw guide cap (2):1',#17090,#17092,
'Jaw guide cap (2):1');
#384=NEXT_ASSEMBLY_USAGE_OCCURRENCE('Jaw guide cap (3):1',
'Jaw guide cap (3):1','Jaw guide cap (3):1',#17090,#17093,
'Jaw guide cap (3):1');
#385=NEXT_ASSEMBLY_USAGE_OCCURRENCE('Right screw nut:1',
'Right screw nut:1','Right screw nut:1',#17090,#17094,
'Right screw nut:1');
#386=NEXT_ASSEMBLY_USAGE_OCCURRENCE('Right jaw plate:1',
'Right jaw plate:1','Right jaw plate:1',#17090,#17095,
'Right jaw plate:1');
#387=NEXT_ASSEMBLY_USAGE_OCCURRENCE(
'Linear Ball Bushing - 12 x 21 x 30 mm:4',
'Linear Ball Bushing - 12 x 21 x 30 mm:4',
'Linear Ball Bushing - 12 x 21 x 30 mm:4',#17090,#17096,
'Linear Ball Bushing - 12 x 21 x 30 mm:4');
#388=NEXT_ASSEMBLY_USAGE_OCCURRENCE(
'Linear Ball Bushing - 12 x 21 x 30 mm:5',
'Linear Ball Bushing - 12 x 21 x 30 mm:5',
'Linear Ball Bushing - 12 x 21 x 30 mm:5',#17090,#17096,
'Linear Ball Bushing - 12 x 21 x 30 mm:5');
#389=NEXT_ASSEMBLY_USAGE_OCCURRENCE('M4x10 Cap Screw:28',
'M4x10 Cap Screw:28','M4x10 Cap Screw:28',#17090,#17099,
'M4x10 Cap Screw:28');
#390=NEXT_ASSEMBLY_USAGE_OCCURRENCE('M4x10 Cap Screw:29',
'M4x10 Cap Screw:29','M4x10 Cap Screw:29',#17090,#17099,
'M4x10 Cap Screw:29');
#391=NEXT_ASSEMBLY_USAGE_OCCURRENCE('M4x10 Cap Screw:30',
'M4x10 Cap Screw:30','M4x10 Cap Screw:30',#17090,#17099,
'M4x10 Cap Screw:30');
#392=NEXT_ASSEMBLY_USAGE_OCCURRENCE('M4x10 Cap Screw:31',
'M4x10 Cap Screw:31','M4x10 Cap Screw:31',#17090,#17099,
'M4x10 Cap Screw:31');
#393=NEXT_ASSEMBLY_USAGE_OCCURRENCE('M4x10 Cap Screw:32',
'M4x10 Cap Screw:32','M4x10 Cap Screw:32',#17090,#17099,
'M4x10 Cap Screw:32');
#394=NEXT_ASSEMBLY_USAGE_OCCURRENCE('M4x10 Cap Screw:33',
'M4x10 Cap Screw:33','M4x10 Cap Screw:33',#17090,#17099,
'M4x10 Cap Screw:33');
#395=NEXT_ASSEMBLY_USAGE_OCCURRENCE('M4x10 Cap Screw:34',
'M4x10 Cap Screw:34','M4x10 Cap Screw:34',#17090,#17099,
'M4x10 Cap Screw:34');
#396=NEXT_ASSEMBLY_USAGE_OCCURRENCE('M4x10 Cap Screw:35',
'M4x10 Cap Screw:35','M4x10 Cap Screw:35',#17090,#17099,
'M4x10 Cap Screw:35');
#397=NEXT_ASSEMBLY_USAGE_OCCURRENCE('M4x10 Cap Screw:36',
'M4x10 Cap Screw:36','M4x10 Cap Screw:36',#17090,#17099,
'M4x10 Cap Screw:36');
#398=NEXT_ASSEMBLY_USAGE_OCCURRENCE('M4x10 Cap Screw:37',
'M4x10 Cap Screw:37','M4x10 Cap Screw:37',#17090,#17099,
'M4x10 Cap Screw:37');
#399=NEXT_ASSEMBLY_USAGE_OCCURRENCE('Cap Screw - M4x16:18',
'Cap Screw - M4x16:18','Cap Screw - M4x16:18',#17090,#17108,
'Cap Screw - M4x16:18');
#400=NEXT_ASSEMBLY_USAGE_OCCURRENCE('Cap Screw - M4x16:19',
'Cap Screw - M4x16:19','Cap Screw - M4x16:19',#17090,#17108,
'Cap Screw - M4x16:19');
#401=NEXT_ASSEMBLY_USAGE_OCCURRENCE('Cap Screw - M4x16:20',
'Cap Screw - M4x16:20','Cap Screw - M4x16:20',#17090,#17108,
'Cap Screw - M4x16:20');
#402=NEXT_ASSEMBLY_USAGE_OCCURRENCE('Cap Screw - M4x16:21',
'Cap Screw - M4x16:21','Cap Screw - M4x16:21',#17090,#17108,
'Cap Screw - M4x16:21');
#403=NEXT_ASSEMBLY_USAGE_OCCURRENCE('Base:1','Base:1','Base:1',#17063,#17064,
'Base:1');
#404=NEXT_ASSEMBLY_USAGE_OCCURRENCE('Foot strip:1','Foot strip:1',
'Foot strip:1',#17063,#17065,'Foot strip:1');
#405=NEXT_ASSEMBLY_USAGE_OCCURRENCE('Foot strip (1):1',
'Foot strip (1):1','Foot strip (1):1',#17063,#17066,'Foot strip (1):1');
#406=NEXT_ASSEMBLY_USAGE_OCCURRENCE('Guide shaft support:1',
'Guide shaft support:1','Guide shaft support:1',#17063,#17067,
'Guide shaft support:1');
#407=NEXT_ASSEMBLY_USAGE_OCCURRENCE('Guide shaft support (1):1',
'Guide shaft support (1):1','Guide shaft support (1):1',#17063,#17068,
'Guide shaft support (1):1');
#408=NEXT_ASSEMBLY_USAGE_OCCURRENCE('Guide shaft support (2):1',
'Guide shaft support (2):1','Guide shaft support (2):1',#17063,#17069,
'Guide shaft support (2):1');
#409=NEXT_ASSEMBLY_USAGE_OCCURRENCE('Guide shaft support (3):1',
'Guide shaft support (3):1','Guide shaft support (3):1',#17063,#17070,
'Guide shaft support (3):1');
#410=NEXT_ASSEMBLY_USAGE_OCCURRENCE('Screw bearing post:1',
'Screw bearing post:1','Screw bearing post:1',#17063,#17071,
'Screw bearing post:1');
#411=NEXT_ASSEMBLY_USAGE_OCCURRENCE('Bearing cap:1','Bearing cap:1',
'Bearing cap:1',#17063,#17072,'Bearing cap:1');
#412=NEXT_ASSEMBLY_USAGE_OCCURRENCE('Bearing cap (1):1',
'Bearing cap (1):1','Bearing cap (1):1',#17063,#17073,
'Bearing cap (1):1');
#413=NEXT_ASSEMBLY_USAGE_OCCURRENCE('Screw bearing post (1):1',
'Screw bearing post (1):1','Screw bearing post (1):1',#17063,#17074,
'Screw bearing post (1):1');
#414=NEXT_ASSEMBLY_USAGE_OCCURRENCE('Bearing cap (2):1',
'Bearing cap (2):1','Bearing cap (2):1',#17063,#17075,
'Bearing cap (2):1');
#415=NEXT_ASSEMBLY_USAGE_OCCURRENCE('Bearing cap (3):1',
'Bearing cap (3):1','Bearing cap (3):1',#17063,#17076,
'Bearing cap (3):1');
#416=NEXT_ASSEMBLY_USAGE_OCCURRENCE(
'Precision Shaft - 12 mm Diameter, 300 mm Long:2',
'Precision Shaft - 12 mm Diameter, 300 mm Long:2',
'Precision Shaft - 12 mm Diameter, 300 mm Long:2',#17063,#17077,
'Precision Shaft - 12 mm Diameter, 300 mm Long:2');
#417=NEXT_ASSEMBLY_USAGE_OCCURRENCE('Cap Screw - M4x16:2',
'Cap Screw - M4x16:2','Cap Screw - M4x16:2',#17063,#17108,
'Cap Screw - M4x16:2');
#418=NEXT_ASSEMBLY_USAGE_OCCURRENCE('Cap Screw - M4x16:3',
'Cap Screw - M4x16:3','Cap Screw - M4x16:3',#17063,#17108,
'Cap Screw - M4x16:3');
#419=NEXT_ASSEMBLY_USAGE_OCCURRENCE('Socket Set Screw - M4x6:2',
'Socket Set Screw - M4x6:2','Socket Set Screw - M4x6:2',#17063,#17109,
'Socket Set Screw - M4x6:2');
#420=NEXT_ASSEMBLY_USAGE_OCCURRENCE('Cap Screw - M4x16:4',
'Cap Screw - M4x16:4','Cap Screw - M4x16:4',#17063,#17108,
'Cap Screw - M4x16:4');
#421=NEXT_ASSEMBLY_USAGE_OCCURRENCE('Cap Screw - M4x16:5',
'Cap Screw - M4x16:5','Cap Screw - M4x16:5',#17063,#17108,
'Cap Screw - M4x16:5');
#422=NEXT_ASSEMBLY_USAGE_OCCURRENCE('Socket Set Screw - M4x6:3',
'Socket Set Screw - M4x6:3','Socket Set Screw - M4x6:3',#17063,#17109,
'Socket Set Screw - M4x6:3');
#423=NEXT_ASSEMBLY_USAGE_OCCURRENCE(
'Precision Shaft - 12 mm Diameter, 300 mm Long:3',
'Precision Shaft - 12 mm Diameter, 300 mm Long:3',
'Precision Shaft - 12 mm Diameter, 300 mm Long:3',#17063,#17077,
'Precision Shaft - 12 mm Diameter, 300 mm Long:3');
#424=NEXT_ASSEMBLY_USAGE_OCCURRENCE('Cap Screw - M4x16:6',
'Cap Screw - M4x16:6','Cap Screw - M4x16:6',#17063,#17108,
'Cap Screw - M4x16:6');
#425=NEXT_ASSEMBLY_USAGE_OCCURRENCE('Cap Screw - M4x16:7',
'Cap Screw - M4x16:7','Cap Screw - M4x16:7',#17063,#17108,
'Cap Screw - M4x16:7');
#426=NEXT_ASSEMBLY_USAGE_OCCURRENCE('Socket Set Screw - M4x6:4',
'Socket Set Screw - M4x6:4','Socket Set Screw - M4x6:4',#17063,#17109,
'Socket Set Screw - M4x6:4');
#427=NEXT_ASSEMBLY_USAGE_OCCURRENCE('Cap Screw - M4x16:8',
'Cap Screw - M4x16:8','Cap Screw - M4x16:8',#17063,#17108,
'Cap Screw - M4x16:8');
#428=NEXT_ASSEMBLY_USAGE_OCCURRENCE('Cap Screw - M4x16:9',
'Cap Screw - M4x16:9','Cap Screw - M4x16:9',#17063,#17108,
'Cap Screw - M4x16:9');
#429=NEXT_ASSEMBLY_USAGE_OCCURRENCE('Socket Set Screw - M4x6:5',
'Socket Set Screw - M4x6:5','Socket Set Screw - M4x6:5',#17063,#17109,
'Socket Set Screw - M4x6:5');
#430=NEXT_ASSEMBLY_USAGE_OCCURRENCE('Cap Screw - M4x16:10',
'Cap Screw - M4x16:10','Cap Screw - M4x16:10',#17063,#17108,
'Cap Screw - M4x16:10');
#431=NEXT_ASSEMBLY_USAGE_OCCURRENCE('Cap Screw - M4x16:11',
'Cap Screw - M4x16:11','Cap Screw - M4x16:11',#17063,#17108,
'Cap Screw - M4x16:11');
#432=NEXT_ASSEMBLY_USAGE_OCCURRENCE(
'Sealed Ball Bearing - 12 x 32 x 10 mm:2',
'Sealed Ball Bearing - 12 x 32 x 10 mm:2',
'Sealed Ball Bearing - 12 x 32 x 10 mm:2',#17063,#17078,
'Sealed Ball Bearing - 12 x 32 x 10 mm:2');
#433=NEXT_ASSEMBLY_USAGE_OCCURRENCE('M4x10 Cap Screw:2',
'M4x10 Cap Screw:2','M4x10 Cap Screw:2',#17063,#17099,
'M4x10 Cap Screw:2');
#434=NEXT_ASSEMBLY_USAGE_OCCURRENCE('M4x10 Cap Screw:3',
'M4x10 Cap Screw:3','M4x10 Cap Screw:3',#17063,#17099,
'M4x10 Cap Screw:3');
#435=NEXT_ASSEMBLY_USAGE_OCCURRENCE('M4x10 Cap Screw:4',
'M4x10 Cap Screw:4','M4x10 Cap Screw:4',#17063,#17099,
'M4x10 Cap Screw:4');
#436=NEXT_ASSEMBLY_USAGE_OCCURRENCE('M4x10 Cap Screw:5',
'M4x10 Cap Screw:5','M4x10 Cap Screw:5',#17063,#17099,
'M4x10 Cap Screw:5');
#437=NEXT_ASSEMBLY_USAGE_OCCURRENCE('M4x10 Cap Screw:6',
'M4x10 Cap Screw:6','M4x10 Cap Screw:6',#17063,#17099,
'M4x10 Cap Screw:6');
#438=NEXT_ASSEMBLY_USAGE_OCCURRENCE('M4x10 Cap Screw:7',
'M4x10 Cap Screw:7','M4x10 Cap Screw:7',#17063,#17099,
'M4x10 Cap Screw:7');
#439=NEXT_ASSEMBLY_USAGE_OCCURRENCE('M4x10 Cap Screw:8',
'M4x10 Cap Screw:8','M4x10 Cap Screw:8',#17063,#17099,
'M4x10 Cap Screw:8');
#440=NEXT_ASSEMBLY_USAGE_OCCURRENCE('M4x10 Cap Screw:9',
'M4x10 Cap Screw:9','M4x10 Cap Screw:9',#17063,#17099,
'M4x10 Cap Screw:9');
#441=NEXT_ASSEMBLY_USAGE_OCCURRENCE('Cap Screw - M4x16:12',
'Cap Screw - M4x16:12','Cap Screw - M4x16:12',#17063,#17108,
'Cap Screw - M4x16:12');
#442=NEXT_ASSEMBLY_USAGE_OCCURRENCE('Cap Screw - M4x16:13',
'Cap Screw - M4x16:13','Cap Screw - M4x16:13',#17063,#17108,
'Cap Screw - M4x16:13');
#443=NEXT_ASSEMBLY_USAGE_OCCURRENCE(
'Sealed Ball Bearing - 12 x 32 x 10 mm:3',
'Sealed Ball Bearing - 12 x 32 x 10 mm:3',
'Sealed Ball Bearing - 12 x 32 x 10 mm:3',#17063,#17078,
'Sealed Ball Bearing - 12 x 32 x 10 mm:3');
#444=NEXT_ASSEMBLY_USAGE_OCCURRENCE('M4x10 Cap Screw:10',
'M4x10 Cap Screw:10','M4x10 Cap Screw:10',#17063,#17099,
'M4x10 Cap Screw:10');
#445=NEXT_ASSEMBLY_USAGE_OCCURRENCE('M4x10 Cap Screw:11',
'M4x10 Cap Screw:11','M4x10 Cap Screw:11',#17063,#17099,
'M4x10 Cap Screw:11');
#446=NEXT_ASSEMBLY_USAGE_OCCURRENCE('M4x10 Cap Screw:12',
'M4x10 Cap Screw:12','M4x10 Cap Screw:12',#17063,#17099,
'M4x10 Cap Screw:12');
#447=NEXT_ASSEMBLY_USAGE_OCCURRENCE('M4x10 Cap Screw:13',
'M4x10 Cap Screw:13','M4x10 Cap Screw:13',#17063,#17099,
'M4x10 Cap Screw:13');
#448=NEXT_ASSEMBLY_USAGE_OCCURRENCE('M4x10 Cap Screw:14',
'M4x10 Cap Screw:14','M4x10 Cap Screw:14',#17063,#17099,
'M4x10 Cap Screw:14');
#449=NEXT_ASSEMBLY_USAGE_OCCURRENCE('M4x10 Cap Screw:15',
'M4x10 Cap Screw:15','M4x10 Cap Screw:15',#17063,#17099,
'M4x10 Cap Screw:15');
#450=NEXT_ASSEMBLY_USAGE_OCCURRENCE('M4x10 Cap Screw:16',
'M4x10 Cap Screw:16','M4x10 Cap Screw:16',#17063,#17099,
'M4x10 Cap Screw:16');
#451=NEXT_ASSEMBLY_USAGE_OCCURRENCE('M4x10 Cap Screw:17',
'M4x10 Cap Screw:17','M4x10 Cap Screw:17',#17063,#17099,
'M4x10 Cap Screw:17');
#452=NEXT_ASSEMBLY_USAGE_OCCURRENCE('Opposed M12 x 3 screw envelope:1',
'Opposed M12 x 3 screw envelope:1','Opposed M12 x 3 screw envelope:1',#17100,
#17101,'Opposed M12 x 3 screw envelope:1');
#453=NEXT_ASSEMBLY_USAGE_OCCURRENCE('Outer bearing sleeve:1',
'Outer bearing sleeve:1','Outer bearing sleeve:1',#17100,#17102,
'Outer bearing sleeve:1');
#454=NEXT_ASSEMBLY_USAGE_OCCURRENCE('Outer bearing sleeve (1):1',
'Outer bearing sleeve (1):1','Outer bearing sleeve (1):1',#17100,#17103,
'Outer bearing sleeve (1):1');
#455=NEXT_ASSEMBLY_USAGE_OCCURRENCE('Handwheel:1','Handwheel:1',
'Handwheel:1',#17100,#17104,'Handwheel:1');
#456=NEXT_ASSEMBLY_USAGE_OCCURRENCE('Shaft keeper:1','Shaft keeper:1',
'Shaft keeper:1',#17100,#17105,'Shaft keeper:1');
#457=NEXT_ASSEMBLY_USAGE_OCCURRENCE('Shaft keeper (1):1',
'Shaft keeper (1):1','Shaft keeper (1):1',#17100,#17106,
'Shaft keeper (1):1');
#458=NEXT_ASSEMBLY_USAGE_OCCURRENCE('Right end collar:1',
'Right end collar:1','Right end collar:1',#17100,#17107,
'Right end collar:1');
#459=NEXT_ASSEMBLY_USAGE_OCCURRENCE('Socket Set Screw - M4x6:6',
'Socket Set Screw - M4x6:6','Socket Set Screw - M4x6:6',#17100,#17109,
'Socket Set Screw - M4x6:6');
#460=NEXT_ASSEMBLY_USAGE_OCCURRENCE('Cap Screw - M4x16:22',
'Cap Screw - M4x16:22','Cap Screw - M4x16:22',#17100,#17108,
'Cap Screw - M4x16:22');
#461=NEXT_ASSEMBLY_USAGE_OCCURRENCE('Cap Screw - M4x16:23',
'Cap Screw - M4x16:23','Cap Screw - M4x16:23',#17100,#17108,
'Cap Screw - M4x16:23');
#462=NEXT_ASSEMBLY_USAGE_OCCURRENCE('Socket Set Screw - M4x6:7',
'Socket Set Screw - M4x6:7','Socket Set Screw - M4x6:7',#17100,#17109,
'Socket Set Screw - M4x6:7');
#463=NEXT_ASSEMBLY_USAGE_OCCURRENCE('Base, shafts and bearings:1',
'Base, shafts and bearings:1','Base, shafts and bearings:1',#17062,#17063,
'Base, shafts and bearings:1');
#464=NEXT_ASSEMBLY_USAGE_OCCURRENCE('Left moving jaw:1',
'Left moving jaw:1','Left moving jaw:1',#17062,#17084,
'Left moving jaw:1');
#465=NEXT_ASSEMBLY_USAGE_OCCURRENCE('Right moving jaw:1',
'Right moving jaw:1','Right moving jaw:1',#17062,#17090,
'Right moving jaw:1');
#466=NEXT_ASSEMBLY_USAGE_OCCURRENCE('Opposed screw and handwheel:1',
'Opposed screw and handwheel:1','Opposed screw and handwheel:1',#17062,
#17100,'Opposed screw and handwheel:1');
#467=SPHERICAL_SURFACE('',#9996,0.29765);
#468=SPHERICAL_SURFACE('',#9998,0.29765);
#469=SPHERICAL_SURFACE('',#10000,0.29765);
#470=SPHERICAL_SURFACE('',#10002,0.29765);
#471=SPHERICAL_SURFACE('',#10004,0.29765);
#472=SPHERICAL_SURFACE('',#10006,0.29765);
#473=SPHERICAL_SURFACE('',#10008,0.29765);
#474=SPHERICAL_SURFACE('',#10011,0.309556);
#475=SPHERICAL_SURFACE('',#10027,0.309556);
#476=SPHERICAL_SURFACE('',#10032,0.309556);
#477=SPHERICAL_SURFACE('',#10038,0.309556);
#478=SPHERICAL_SURFACE('',#10043,0.309556);
#479=SPHERICAL_SURFACE('',#10048,0.309556);
#480=SPHERICAL_SURFACE('',#10056,0.309556);
#481=TOROIDAL_SURFACE('',#9956,1.1,0.309556);
#482=TOROIDAL_SURFACE('',#9976,1.1,0.309556);
#483=CONICAL_SURFACE('',#9945,0.55,0.785398163397448);
#484=CONICAL_SURFACE('',#9951,0.55,0.785398163397441);
#485=CONICAL_SURFACE('',#9967,0.63,0.785398163397448);
#486=CONICAL_SURFACE('',#9974,0.63,0.785398163397448);
#487=CONICAL_SURFACE('',#9987,1.57,0.785398163397449);
#488=CONICAL_SURFACE('',#9991,1.57,0.785398163397449);
#489=CONICAL_SURFACE('',#10493,0.325,0.785398163397448);
#490=CONICAL_SURFACE('',#10497,0.335,0.785398163397448);
#491=CONICAL_SURFACE('',#10501,0.21,0.463647609000806);
#492=CONICAL_SURFACE('',#10606,0.325,0.785398163397448);
#493=CONICAL_SURFACE('',#10610,0.335,0.785398163397448);
#494=CONICAL_SURFACE('',#10614,0.21,0.463647609000806);
#495=CONICAL_SURFACE('',#10618,0.18,0.785398163397448);
#496=CONICAL_SURFACE('',#10681,0.185,0.785398163397449);
#497=CONICAL_SURFACE('',#10685,0.1625,0.785398163397449);
#498=B_SPLINE_CURVE_WITH_KNOTS('',3,(#13857,#13858,#13859,#13860,#13861,
#13862),.UNSPECIFIED.,.F.,.F.,(4,2,4),(0.63543032495593,0.687528937234027,
0.750024497760672),.UNSPECIFIED.);
#499=B_SPLINE_CURVE_WITH_KNOTS('',3,(#13866,#13867,#13868,#13869,#13870,
#13871),.UNSPECIFIED.,.F.,.F.,(4,2,4),(0.250008165920224,0.312503726446869,
0.364602338724965),.UNSPECIFIED.);
#500=B_SPLINE_CURVE_WITH_KNOTS('',3,(#13872,#13873,#13874,#13875,#13876,
#13877),.UNSPECIFIED.,.F.,.F.,(4,2,4),(0.135413993115483,0.187512605393579,
0.250008165920224),.UNSPECIFIED.);
#501=B_SPLINE_CURVE_WITH_KNOTS('',3,(#13878,#13879,#13880,#13881,#13882,
#13883),.UNSPECIFIED.,.F.,.F.,(4,2,4),(0.750024497760672,0.812520058287317,
0.864618670565412),.UNSPECIFIED.);
#502=B_SPLINE_CURVE_WITH_KNOTS('',3,(#13973,#13974,#13975,#13976,#13977,
#13978),.UNSPECIFIED.,.F.,.F.,(4,2,4),(0.635430324955931,0.687528937234027,
0.750024497760672),.UNSPECIFIED.);
#503=B_SPLINE_CURVE_WITH_KNOTS('',3,(#13982,#13983,#13984,#13985,#13986,
#13987),.UNSPECIFIED.,.F.,.F.,(4,2,4),(0.250008165920224,0.312503726446869,
0.364602338724963),.UNSPECIFIED.);
#504=B_SPLINE_CURVE_WITH_KNOTS('',3,(#13988,#13989,#13990,#13991,#13992,
#13993),.UNSPECIFIED.,.F.,.F.,(4,2,4),(0.135413993115483,0.187512605393579,
0.250008165920224),.UNSPECIFIED.);
#505=B_SPLINE_CURVE_WITH_KNOTS('',3,(#13994,#13995,#13996,#13997,#13998,
#13999),.UNSPECIFIED.,.F.,.F.,(4,2,4),(0.750024497760672,0.812520058287317,
0.864618670565414),.UNSPECIFIED.);
#506=B_SPLINE_CURVE_WITH_KNOTS('',3,(#14089,#14090,#14091,#14092,#14093,
#14094),.UNSPECIFIED.,.F.,.F.,(4,2,4),(0.635430324955929,0.687528937234027,
0.750024497760672),.UNSPECIFIED.);
#507=B_SPLINE_CURVE_WITH_KNOTS('',3,(#14098,#14099,#14100,#14101,#14102,
#14103),.UNSPECIFIED.,.F.,.F.,(4,2,4),(0.250008165920224,0.312503726446869,
0.364602338724966),.UNSPECIFIED.);
#508=B_SPLINE_CURVE_WITH_KNOTS('',3,(#14104,#14105,#14106,#14107,#14108,
#14109),.UNSPECIFIED.,.F.,.F.,(4,2,4),(0.135413993115482,0.187512605393579,
0.250008165920224),.UNSPECIFIED.);
#509=B_SPLINE_CURVE_WITH_KNOTS('',3,(#14110,#14111,#14112,#14113,#14114,
#14115),.UNSPECIFIED.,.F.,.F.,(4,2,4),(0.750024497760672,0.812520058287317,
0.864618670565413),.UNSPECIFIED.);
#510=B_SPLINE_CURVE_WITH_KNOTS('',3,(#14205,#14206,#14207,#14208,#14209,
#14210),.UNSPECIFIED.,.F.,.F.,(4,2,4),(0.635430324955931,0.687528937234027,
0.750024497760672),.UNSPECIFIED.);
#511=B_SPLINE_CURVE_WITH_KNOTS('',3,(#14214,#14215,#14216,#14217,#14218,
#14219),.UNSPECIFIED.,.F.,.F.,(4,2,4),(0.250008165920224,0.312503726446869,
0.364602338724964),.UNSPECIFIED.);
#512=B_SPLINE_CURVE_WITH_KNOTS('',3,(#14220,#14221,#14222,#14223,#14224,
#14225),.UNSPECIFIED.,.F.,.F.,(4,2,4),(0.135413993115483,0.187512605393579,
0.250008165920224),.UNSPECIFIED.);
#513=B_SPLINE_CURVE_WITH_KNOTS('',3,(#14226,#14227,#14228,#14229,#14230,
#14231),.UNSPECIFIED.,.F.,.F.,(4,2,4),(0.750024497760672,0.812520058287317,
0.864618670565414),.UNSPECIFIED.);
#514=B_SPLINE_CURVE_WITH_KNOTS('',3,(#14785,#14786,#14787,#14788,#14789,
#14790,#14791,#14792,#14793,#14794,#14795,#14796,#14797,#14798,#14799,#14800,
#14801,#14802,#14803,#14804,#14805,#14806),.UNSPECIFIED.,.F.,.F.,(4,2,2,
2,2,2,2,2,2,2,4),(0.0591825211272536,0.157966726598481,0.236950089897721,
0.315933453196962,0.391576304923761,0.46721915665056,0.54286200837736,0.618504860104159,
0.697488223403399,0.77647158670264,0.875255792173867),.UNSPECIFIED.);
#515=B_SPLINE_CURVE_WITH_KNOTS('',3,(#14810,#14811,#14812,#14813,#14814,
#14815,#14816,#14817,#14818,#14819,#14820,#14821,#14822,#14823,#14824,#14825,
#14826,#14827,#14828,#14829,#14830,#14831),.UNSPECIFIED.,.F.,.F.,(4,2,2,
2,2,2,2,2,2,2,4),(0.0581119756758434,0.106553146291161,0.213106292582322,
0.30849933801665,0.386091982889075,0.4636846277615,0.541277272633925,0.61886991750635,
0.714262962940678,0.820816109231839,0.869257279847157),.UNSPECIFIED.);
#516=B_SPLINE_CURVE_WITH_KNOTS('',3,(#14837,#14838,#14839,#14840,#14841,
#14842,#14843,#14844,#14845,#14846,#14847,#14848,#14849,#14850,#14851,#14852,
#14853,#14854,#14855,#14856,#14857,#14858),.UNSPECIFIED.,.F.,.F.,(4,2,2,
2,2,2,2,2,2,2,4),(0.0581119756758434,0.106553146291161,0.213106292582322,
0.30849933801665,0.386091982889075,0.4636846277615,0.541277272633925,0.61886991750635,
0.714262962940679,0.820816109231839,0.869257279847157),.UNSPECIFIED.);
#517=B_SPLINE_CURVE_WITH_KNOTS('',3,(#14862,#14863,#14864,#14865,#14866,
#14867,#14868,#14869,#14870,#14871,#14872,#14873,#14874,#14875,#14876,#14877,
#14878,#14879,#14880,#14881,#14882,#14883),.UNSPECIFIED.,.F.,.F.,(4,2,2,
2,2,2,2,2,2,2,4),(0.0581119756758433,0.106553146291161,0.213106292582322,
0.308499338016649,0.386091982889075,0.4636846277615,0.541277272633925,0.61886991750635,
0.714262962940678,0.820816109231839,0.869257279847157),.UNSPECIFIED.);
#518=B_SPLINE_CURVE_WITH_KNOTS('',3,(#14892,#14893,#14894,#14895,#14896,
#14897,#14898,#14899,#14900,#14901,#14902,#14903,#14904,#14905,#14906,#14907,
#14908,#14909,#14910,#14911,#14912,#14913),.UNSPECIFIED.,.F.,.F.,(4,2,2,
2,2,2,2,2,2,2,4),(0.0581119756758433,0.106553146291161,0.213106292582322,
0.30849933801665,0.386091982889075,0.4636846277615,0.541277272633925,0.61886991750635,
0.714262962940678,0.820816109231839,0.869257279847157),.UNSPECIFIED.);
#519=B_SPLINE_CURVE_WITH_KNOTS('',3,(#14917,#14918,#14919,#14920,#14921,
#14922,#14923,#14924,#14925,#14926,#14927,#14928,#14929,#14930,#14931,#14932,
#14933,#14934,#14935,#14936,#14937,#14938),.UNSPECIFIED.,.F.,.F.,(4,2,2,
2,2,2,2,2,2,2,4),(0.0581119756758434,0.106553146291161,0.213106292582322,
0.30849933801665,0.386091982889075,0.4636846277615,0.541277272633925,0.61886991750635,
0.714262962940678,0.820816109231839,0.869257279847157),.UNSPECIFIED.);
#520=B_SPLINE_CURVE_WITH_KNOTS('',3,(#14942,#14943,#14944,#14945,#14946,
#14947,#14948,#14949,#14950,#14951,#14952,#14953,#14954,#14955,#14956,#14957,
#14958,#14959,#14960,#14961,#14962,#14963),.UNSPECIFIED.,.F.,.F.,(4,2,2,
2,2,2,2,2,2,2,4),(0.0581119756758434,0.106553146291161,0.213106292582322,
0.30849933801665,0.386091982889075,0.4636846277615,0.541277272633925,0.61886991750635,
0.714262962940678,0.820816109231839,0.869257279847157),.UNSPECIFIED.);
#521=B_SPLINE_CURVE_WITH_KNOTS('',3,(#14967,#14968,#14969,#14970,#14971,
#14972,#14973,#14974,#14975,#14976,#14977,#14978,#14979,#14980,#14981,#14982,
#14983,#14984,#14985,#14986,#14987,#14988),.UNSPECIFIED.,.F.,.F.,(4,2,2,
2,2,2,2,2,2,2,4),(0.0581119756758433,0.106553146291161,0.213106292582322,
0.30849933801665,0.386091982889075,0.4636846277615,0.541277272633925,0.61886991750635,
0.714262962940678,0.820816109231839,0.869257279847157),.UNSPECIFIED.);
#522=B_SPLINE_CURVE_WITH_KNOTS('',3,(#14996,#14997,#14998,#14999,#15000,
#15001,#15002,#15003,#15004,#15005,#15006,#15007,#15008,#15009,#15010,#15011,
#15012,#15013,#15014,#15015,#15016,#15017),.UNSPECIFIED.,.F.,.F.,(4,2,2,
2,2,2,2,2,2,2,4),(0.0591825211272536,0.157966726598481,0.236950089897721,
0.315933453196962,0.391576304923761,0.467219156650561,0.54286200837736,
0.618504860104159,0.697488223403399,0.77647158670264,0.875255792173867),
 .UNSPECIFIED.);
#523=B_SPLINE_CURVE_WITH_KNOTS('',3,(#15025,#15026,#15027,#15028,#15029,
#15030,#15031,#15032,#15033,#15034,#15035,#15036,#15037,#15038,#15039,#15040,
#15041,#15042,#15043,#15044,#15045,#15046),.UNSPECIFIED.,.F.,.F.,(4,2,2,
2,2,2,2,2,2,2,4),(0.0591825211272536,0.157966726598481,0.236950089897722,
0.315933453196962,0.391576304923761,0.467219156650561,0.54286200837736,
0.618504860104159,0.697488223403399,0.77647158670264,0.875255792173867),
 .UNSPECIFIED.);
#524=B_SPLINE_CURVE_WITH_KNOTS('',3,(#15056,#15057,#15058,#15059,#15060,
#15061,#15062,#15063,#15064,#15065,#15066,#15067,#15068,#15069,#15070,#15071,
#15072,#15073,#15074,#15075,#15076,#15077),.UNSPECIFIED.,.F.,.F.,(4,2,2,
2,2,2,2,2,2,2,4),(0.0591825211272536,0.157966726598481,0.236950089897721,
0.315933453196962,0.391576304923761,0.46721915665056,0.54286200837736,0.618504860104159,
0.697488223403399,0.77647158670264,0.875255792173867),.UNSPECIFIED.);
#525=B_SPLINE_CURVE_WITH_KNOTS('',3,(#15085,#15086,#15087,#15088,#15089,
#15090,#15091,#15092,#15093,#15094,#15095,#15096,#15097,#15098,#15099,#15100,
#15101,#15102,#15103,#15104,#15105,#15106),.UNSPECIFIED.,.F.,.F.,(4,2,2,
2,2,2,2,2,2,2,4),(0.0591825211272536,0.157966726598481,0.236950089897721,
0.315933453196962,0.391576304923761,0.46721915665056,0.542862008377359,
0.618504860104159,0.697488223403399,0.776471586702639,0.875255792173867),
 .UNSPECIFIED.);
#526=B_SPLINE_CURVE_WITH_KNOTS('',3,(#15114,#15115,#15116,#15117,#15118,
#15119,#15120,#15121,#15122,#15123,#15124,#15125,#15126,#15127,#15128,#15129,
#15130,#15131,#15132,#15133,#15134,#15135),.UNSPECIFIED.,.F.,.F.,(4,2,2,
2,2,2,2,2,2,2,4),(0.0591825211272536,0.157966726598481,0.236950089897721,
0.315933453196962,0.391576304923761,0.46721915665056,0.54286200837736,0.618504860104159,
0.697488223403399,0.77647158670264,0.875255792173867),.UNSPECIFIED.);
#527=B_SPLINE_CURVE_WITH_KNOTS('',3,(#15144,#15145,#15146,#15147,#15148,
#15149,#15150,#15151,#15152,#15153,#15154,#15155,#15156,#15157,#15158,#15159,
#15160,#15161,#15162,#15163,#15164,#15165),.UNSPECIFIED.,.F.,.F.,(4,2,2,
2,2,2,2,2,2,2,4),(0.0591825211272536,0.157966726598481,0.236950089897721,
0.315933453196962,0.391576304923761,0.46721915665056,0.542862008377359,
0.618504860104159,0.697488223403399,0.776471586702639,0.875255792173867),
 .UNSPECIFIED.);
#528=B_SPLINE_CURVE_WITH_KNOTS('',3,(#16250,#16251,#16252,#16253,#16254,
#16255),.UNSPECIFIED.,.F.,.F.,(4,2,4),(0.635430324955929,0.687528937234027,
0.750024497760672),.UNSPECIFIED.);
#529=B_SPLINE_CURVE_WITH_KNOTS('',3,(#16259,#16260,#16261,#16262,#16263,
#16264),.UNSPECIFIED.,.F.,.F.,(4,2,4),(0.250008165920224,0.312503726446869,
0.364602338724964),.UNSPECIFIED.);
#530=B_SPLINE_CURVE_WITH_KNOTS('',3,(#16265,#16266,#16267,#16268,#16269,
#16270),.UNSPECIFIED.,.F.,.F.,(4,2,4),(0.135413993115483,0.187512605393579,
0.250008165920224),.UNSPECIFIED.);
#531=B_SPLINE_CURVE_WITH_KNOTS('',3,(#16271,#16272,#16273,#16274,#16275,
#16276),.UNSPECIFIED.,.F.,.F.,(4,2,4),(0.750024497760672,0.812520058287317,
0.864618670565415),.UNSPECIFIED.);
#532=B_SPLINE_CURVE_WITH_KNOTS('',3,(#16280,#16281,#16282,#16283,#16284,
#16285,#16286,#16287,#16288,#16289),.UNSPECIFIED.,.F.,.F.,(4,2,2,2,4),(0.,
0.0622384309821294,0.124476861964259,0.186714529331343,0.248952196698427),
 .UNSPECIFIED.);
#533=B_SPLINE_CURVE_WITH_KNOTS('',3,(#16291,#16292,#16293,#16294,#16295,
#16296,#16297,#16298,#16299,#16300),.UNSPECIFIED.,.F.,.F.,(4,2,2,2,4),(0.74685659009528,
0.809094257462364,0.871331924829448,0.933570355811577,0.995808786793707),
 .UNSPECIFIED.);
#534=B_SPLINE_CURVE_WITH_KNOTS('',3,(#16301,#16302,#16303,#16304,#16305,
#16306,#16307,#16308,#16309,#16310,#16311,#16312,#16313,#16314,#16315,#16316,
#16317,#16318),.UNSPECIFIED.,.F.,.F.,(4,2,2,2,2,2,2,2,4),(0.248952196698427,
0.311189864065511,0.373427531432595,0.435665962414724,0.497904393396853,
0.560142824378983,0.622381255361112,0.684618922728196,0.74685659009528),
 .UNSPECIFIED.);
#535=B_SPLINE_CURVE_WITH_KNOTS('',3,(#16377,#16378,#16379,#16380,#16381,
#16382,#16383,#16384),.UNSPECIFIED.,.F.,.F.,(4,2,2,4),(0.598759573717649,
0.624973342427789,0.687463163426141,0.749952984424493),.UNSPECIFIED.);
#536=B_SPLINE_CURVE_WITH_KNOTS('',3,(#16388,#16389,#16390,#16391,#16392,
#16393,#16394,#16395),.UNSPECIFIED.,.F.,.F.,(4,2,2,4),(0.249984328141498,
0.31247414913985,0.374963970138202,0.401177738848341),.UNSPECIFIED.);
#537=B_SPLINE_CURVE_WITH_KNOTS('',3,(#16396,#16397,#16398,#16399,#16400,
#16401,#16402,#16403),.UNSPECIFIED.,.F.,.F.,(4,2,2,4),(0.0987909174346529,
0.125004686144794,0.187494507143146,0.249984328141498),.UNSPECIFIED.);
#538=B_SPLINE_CURVE_WITH_KNOTS('',3,(#16404,#16405,#16406,#16407,#16408,
#16409,#16410,#16411),.UNSPECIFIED.,.F.,.F.,(4,2,2,4),(0.749952984424493,
0.812442805422846,0.874932626421198,0.901146395131338),.UNSPECIFIED.);
#539=B_SPLINE_CURVE_WITH_KNOTS('',3,(#16415,#16416,#16417,#16418,#16419,
#16420,#16421,#16422,#16423,#16424),.UNSPECIFIED.,.F.,.F.,(4,2,2,2,4),(0.,
0.0622766332261793,0.124553266452359,0.186828302721277,0.249103338990195),
 .UNSPECIFIED.);
#540=B_SPLINE_CURVE_WITH_KNOTS('',3,(#16426,#16427,#16428,#16429,#16430,
#16431,#16432,#16433,#16434,#16435),.UNSPECIFIED.,.F.,.F.,(4,2,2,2,4),(0.747310016970586,
0.809585053239505,0.871860089508423,0.934136722734602,0.996413355960782),
 .UNSPECIFIED.);
#541=B_SPLINE_CURVE_WITH_KNOTS('',3,(#16436,#16437,#16438,#16439,#16440,
#16441,#16442,#16443,#16444,#16445,#16446,#16447,#16448,#16449,#16450,#16451,
#16452,#16453),.UNSPECIFIED.,.F.,.F.,(4,2,2,2,2,2,2,2,4),(0.249103338990195,
0.311378375259114,0.373653411528032,0.435930044754212,0.498206677980391,
0.56048331120657,0.62275994443275,0.685034980701668,0.747310016970586),
 .UNSPECIFIED.);
#542=SHAPE_REPRESENTATION_RELATIONSHIP('SRR','None',#17015,#583);
#543=SHAPE_REPRESENTATION_RELATIONSHIP('SRR','None',#17016,#584);
#544=SHAPE_REPRESENTATION_RELATIONSHIP('SRR','None',#17017,#585);
#545=SHAPE_REPRESENTATION_RELATIONSHIP('SRR','None',#17018,#586);
#546=SHAPE_REPRESENTATION_RELATIONSHIP('SRR','None',#17019,#587);
#547=SHAPE_REPRESENTATION_RELATIONSHIP('SRR','None',#17020,#588);
#548=SHAPE_REPRESENTATION_RELATIONSHIP('SRR','None',#17021,#589);
#549=SHAPE_REPRESENTATION_RELATIONSHIP('SRR','None',#17022,#590);
#550=SHAPE_REPRESENTATION_RELATIONSHIP('SRR','None',#17023,#591);
#551=SHAPE_REPRESENTATION_RELATIONSHIP('SRR','None',#17024,#592);
#552=SHAPE_REPRESENTATION_RELATIONSHIP('SRR','None',#17025,#593);
#553=SHAPE_REPRESENTATION_RELATIONSHIP('SRR','None',#17026,#594);
#554=SHAPE_REPRESENTATION_RELATIONSHIP('SRR','None',#17027,#595);
#555=SHAPE_REPRESENTATION_RELATIONSHIP('SRR','None',#17028,#596);
#556=SHAPE_REPRESENTATION_RELATIONSHIP('SRR','None',#17030,#597);
#557=SHAPE_REPRESENTATION_RELATIONSHIP('SRR','None',#17031,#598);
#558=SHAPE_REPRESENTATION_RELATIONSHIP('SRR','None',#17032,#599);
#559=SHAPE_REPRESENTATION_RELATIONSHIP('SRR','None',#17033,#600);
#560=SHAPE_REPRESENTATION_RELATIONSHIP('SRR','None',#17034,#601);
#561=SHAPE_REPRESENTATION_RELATIONSHIP('SRR','None',#17036,#602);
#562=SHAPE_REPRESENTATION_RELATIONSHIP('SRR','None',#17037,#603);
#563=SHAPE_REPRESENTATION_RELATIONSHIP('SRR','None',#17038,#604);
#564=SHAPE_REPRESENTATION_RELATIONSHIP('SRR','None',#17039,#605);
#565=SHAPE_REPRESENTATION_RELATIONSHIP('SRR','None',#17040,#606);
#566=SHAPE_REPRESENTATION_RELATIONSHIP('SRR','None',#17042,#607);
#567=SHAPE_REPRESENTATION_RELATIONSHIP('SRR','None',#17043,#608);
#568=SHAPE_REPRESENTATION_RELATIONSHIP('SRR','None',#17044,#609);
#569=SHAPE_REPRESENTATION_RELATIONSHIP('SRR','None',#17045,#610);
#570=SHAPE_REPRESENTATION_RELATIONSHIP('SRR','None',#17046,#611);
#571=SHAPE_REPRESENTATION_RELATIONSHIP('SRR','None',#17048,#612);
#572=SHAPE_REPRESENTATION_RELATIONSHIP('SRR','None',#17049,#613);
#573=SHAPE_REPRESENTATION_RELATIONSHIP('SRR','None',#17050,#614);
#574=SHAPE_REPRESENTATION_RELATIONSHIP('SRR','None',#17052,#615);
#575=SHAPE_REPRESENTATION_RELATIONSHIP('SRR','None',#17053,#616);
#576=SHAPE_REPRESENTATION_RELATIONSHIP('SRR','None',#17054,#617);
#577=SHAPE_REPRESENTATION_RELATIONSHIP('SRR','None',#17055,#618);
#578=SHAPE_REPRESENTATION_RELATIONSHIP('SRR','None',#17056,#619);
#579=SHAPE_REPRESENTATION_RELATIONSHIP('SRR','None',#17057,#620);
#580=SHAPE_REPRESENTATION_RELATIONSHIP('SRR','None',#17058,#621);
#581=SHAPE_REPRESENTATION_RELATIONSHIP('SRR','None',#17059,#622);
#582=SHAPE_REPRESENTATION_RELATIONSHIP('SRR','None',#17060,#623);
#583=ADVANCED_BREP_SHAPE_REPRESENTATION('',(#672),#16753);
#584=ADVANCED_BREP_SHAPE_REPRESENTATION('',(#673),#16754);
#585=ADVANCED_BREP_SHAPE_REPRESENTATION('',(#674),#16755);
#586=ADVANCED_BREP_SHAPE_REPRESENTATION('',(#675),#16756);
#587=ADVANCED_BREP_SHAPE_REPRESENTATION('',(#676),#16757);
#588=ADVANCED_BREP_SHAPE_REPRESENTATION('',(#677),#16758);
#589=ADVANCED_BREP_SHAPE_REPRESENTATION('',(#678),#16759);
#590=ADVANCED_BREP_SHAPE_REPRESENTATION('',(#679),#16760);
#591=ADVANCED_BREP_SHAPE_REPRESENTATION('',(#680),#16761);
#592=ADVANCED_BREP_SHAPE_REPRESENTATION('',(#681),#16762);
#593=ADVANCED_BREP_SHAPE_REPRESENTATION('',(#682),#16763);
#594=ADVANCED_BREP_SHAPE_REPRESENTATION('',(#683),#16764);
#595=ADVANCED_BREP_SHAPE_REPRESENTATION('',(#684),#16765);
#596=ADVANCED_BREP_SHAPE_REPRESENTATION('',(#685),#16766);
#597=ADVANCED_BREP_SHAPE_REPRESENTATION('',(#686),#16768);
#598=ADVANCED_BREP_SHAPE_REPRESENTATION('',(#687),#16769);
#599=ADVANCED_BREP_SHAPE_REPRESENTATION('',(#688,#689,#690,#691,#692,#693,
#694),#16770);
#600=ADVANCED_BREP_SHAPE_REPRESENTATION('',(#695),#16771);
#601=ADVANCED_BREP_SHAPE_REPRESENTATION('',(#696,#697),#16772);
#602=ADVANCED_BREP_SHAPE_REPRESENTATION('',(#698),#16774);
#603=ADVANCED_BREP_SHAPE_REPRESENTATION('',(#699),#16775);
#604=ADVANCED_BREP_SHAPE_REPRESENTATION('',(#700),#16776);
#605=ADVANCED_BREP_SHAPE_REPRESENTATION('',(#701),#16777);
#606=ADVANCED_BREP_SHAPE_REPRESENTATION('',(#702),#16778);
#607=ADVANCED_BREP_SHAPE_REPRESENTATION('',(#703),#16780);
#608=ADVANCED_BREP_SHAPE_REPRESENTATION('',(#704),#16781);
#609=ADVANCED_BREP_SHAPE_REPRESENTATION('',(#705),#16782);
#610=ADVANCED_BREP_SHAPE_REPRESENTATION('',(#706),#16783);
#611=ADVANCED_BREP_SHAPE_REPRESENTATION('',(#707),#16784);
#612=ADVANCED_BREP_SHAPE_REPRESENTATION('',(#708),#16786);
#613=ADVANCED_BREP_SHAPE_REPRESENTATION('',(#709),#16787);
#614=ADVANCED_BREP_SHAPE_REPRESENTATION('',(#13),#16788);
#615=ADVANCED_BREP_SHAPE_REPRESENTATION('',(#710),#16790);
#616=ADVANCED_BREP_SHAPE_REPRESENTATION('',(#711),#16791);
#617=ADVANCED_BREP_SHAPE_REPRESENTATION('',(#712),#16792);
#618=ADVANCED_BREP_SHAPE_REPRESENTATION('',(#713),#16793);
#619=ADVANCED_BREP_SHAPE_REPRESENTATION('',(#714),#16794);
#620=ADVANCED_BREP_SHAPE_REPRESENTATION('',(#715),#16795);
#621=ADVANCED_BREP_SHAPE_REPRESENTATION('',(#716),#16796);
#622=ADVANCED_BREP_SHAPE_REPRESENTATION('',(#14),#16797);
#623=ADVANCED_BREP_SHAPE_REPRESENTATION('',(#717),#16798);
#624=STYLED_ITEM('',(#17305),#672);
#625=STYLED_ITEM('',(#17312),#673);
#626=STYLED_ITEM('',(#17312),#674);
#627=STYLED_ITEM('',(#17326),#675);
#628=STYLED_ITEM('',(#17326),#676);
#629=STYLED_ITEM('',(#17326),#677);
#630=STYLED_ITEM('',(#17326),#678);
#631=STYLED_ITEM('',(#17333),#679);
#632=STYLED_ITEM('',(#17326),#680);
#633=STYLED_ITEM('',(#17326),#681);
#634=STYLED_ITEM('',(#17333),#682);
#635=STYLED_ITEM('',(#17326),#683);
#636=STYLED_ITEM('',(#17326),#684);
#637=STYLED_ITEM('',(#17326),#685);
#638=STYLED_ITEM('',(#17326),#686);
#639=STYLED_ITEM('',(#17326),#687);
#640=STYLED_ITEM('',(#17326),#688);
#641=STYLED_ITEM('',(#17326),#689);
#642=STYLED_ITEM('',(#17326),#690);
#643=STYLED_ITEM('',(#17326),#691);
#644=STYLED_ITEM('',(#17326),#692);
#645=STYLED_ITEM('',(#17326),#693);
#646=STYLED_ITEM('',(#17326),#694);
#647=STYLED_ITEM('',(#17326),#695);
#648=STYLED_ITEM('',(#17326),#696);
#649=STYLED_ITEM('',(#17326),#697);
#650=STYLED_ITEM('',(#17305),#698);
#651=STYLED_ITEM('',(#17312),#699);
#652=STYLED_ITEM('',(#17312),#700);
#653=STYLED_ITEM('',(#17333),#701);
#654=STYLED_ITEM('',(#17340),#702);
#655=STYLED_ITEM('',(#17305),#703);
#656=STYLED_ITEM('',(#17312),#704);
#657=STYLED_ITEM('',(#17312),#705);
#658=STYLED_ITEM('',(#17333),#706);
#659=STYLED_ITEM('',(#17319),#707);
#660=STYLED_ITEM('',(#17340),#708);
#661=STYLED_ITEM('',(#17319),#709);
#662=STYLED_ITEM('',(#17333),#13);
#663=STYLED_ITEM('',(#17333),#710);
#664=STYLED_ITEM('',(#17326),#711);
#665=STYLED_ITEM('',(#17326),#712);
#666=STYLED_ITEM('',(#17319),#713);
#667=STYLED_ITEM('',(#17326),#714);
#668=STYLED_ITEM('',(#17326),#715);
#669=STYLED_ITEM('',(#17340),#716);
#670=STYLED_ITEM('',(#17333),#14);
#671=STYLED_ITEM('',(#17333),#717);
#672=MANIFOLD_SOLID_BREP('Body1',#9075);
#673=MANIFOLD_SOLID_BREP('Body1',#9076);
#674=MANIFOLD_SOLID_BREP('Body1',#9077);
#675=MANIFOLD_SOLID_BREP('Body1',#9078);
#676=MANIFOLD_SOLID_BREP('Body1',#9079);
#677=MANIFOLD_SOLID_BREP('Body1',#9080);
#678=MANIFOLD_SOLID_BREP('Body1',#9081);
#679=MANIFOLD_SOLID_BREP('Body1',#9082);
#680=MANIFOLD_SOLID_BREP('Body1',#9083);
#681=MANIFOLD_SOLID_BREP('Body1',#9084);
#682=MANIFOLD_SOLID_BREP('Body1',#9085);
#683=MANIFOLD_SOLID_BREP('Body1',#9086);
#684=MANIFOLD_SOLID_BREP('Body1',#9087);
#685=MANIFOLD_SOLID_BREP('Body1',#9088);
#686=MANIFOLD_SOLID_BREP('Body1',#9089);
#687=MANIFOLD_SOLID_BREP('Body1',#9090);
#688=MANIFOLD_SOLID_BREP('Body1',#9091);
#689=MANIFOLD_SOLID_BREP('Body2',#9092);
#690=MANIFOLD_SOLID_BREP('Body3',#9093);
#691=MANIFOLD_SOLID_BREP('Body4',#9094);
#692=MANIFOLD_SOLID_BREP('Body5',#9095);
#693=MANIFOLD_SOLID_BREP('Body6',#9096);
#694=MANIFOLD_SOLID_BREP('Body7',#9097);
#695=MANIFOLD_SOLID_BREP('Continuous crown cage',#9098);
#696=MANIFOLD_SOLID_BREP('Body1',#9099);
#697=MANIFOLD_SOLID_BREP('Body2',#9100);
#698=MANIFOLD_SOLID_BREP('Body1',#9101);
#699=MANIFOLD_SOLID_BREP('Body1',#9102);
#700=MANIFOLD_SOLID_BREP('Body1',#9103);
#701=MANIFOLD_SOLID_BREP('Body1',#9104);
#702=MANIFOLD_SOLID_BREP('Body1',#9105);
#703=MANIFOLD_SOLID_BREP('Body1',#9106);
#704=MANIFOLD_SOLID_BREP('Body1',#9107);
#705=MANIFOLD_SOLID_BREP('Body1',#9108);
#706=MANIFOLD_SOLID_BREP('Body1',#9109);
#707=MANIFOLD_SOLID_BREP('Body1',#9110);
#708=MANIFOLD_SOLID_BREP('Body1',#9111);
#709=MANIFOLD_SOLID_BREP('Body1',#9112);
#710=MANIFOLD_SOLID_BREP('Body1',#9115);
#711=MANIFOLD_SOLID_BREP('Body1',#9116);
#712=MANIFOLD_SOLID_BREP('Body1',#9117);
#713=MANIFOLD_SOLID_BREP('Body1',#9118);
#714=MANIFOLD_SOLID_BREP('Body1',#9119);
#715=MANIFOLD_SOLID_BREP('Body1',#9120);
#716=MANIFOLD_SOLID_BREP('Body1',#9121);
#717=MANIFOLD_SOLID_BREP('Body1',#9124);
#718=FACE_BOUND('',#1794,.T.);
#719=FACE_BOUND('',#1795,.T.);
#720=FACE_BOUND('',#1796,.T.);
#721=FACE_BOUND('',#1797,.T.);
#722=FACE_BOUND('',#1798,.T.);
#723=FACE_BOUND('',#1799,.T.);
#724=FACE_BOUND('',#1800,.T.);
#725=FACE_BOUND('',#1801,.T.);
#726=FACE_BOUND('',#1802,.T.);
#727=FACE_BOUND('',#1803,.T.);
#728=FACE_BOUND('',#1804,.T.);
#729=FACE_BOUND('',#1805,.T.);
#730=FACE_BOUND('',#1807,.T.);
#731=FACE_BOUND('',#1808,.T.);
#732=FACE_BOUND('',#1809,.T.);
#733=FACE_BOUND('',#1810,.T.);
#734=FACE_BOUND('',#1811,.T.);
#735=FACE_BOUND('',#1812,.T.);
#736=FACE_BOUND('',#1813,.T.);
#737=FACE_BOUND('',#1814,.T.);
#738=FACE_BOUND('',#1815,.T.);
#739=FACE_BOUND('',#1816,.T.);
#740=FACE_BOUND('',#1817,.T.);
#741=FACE_BOUND('',#1818,.T.);
#742=FACE_BOUND('',#1838,.T.);
#743=FACE_BOUND('',#1841,.T.);
#744=FACE_BOUND('',#1843,.T.);
#745=FACE_BOUND('',#1849,.T.);
#746=FACE_BOUND('',#1852,.T.);
#747=FACE_BOUND('',#1854,.T.);
#748=FACE_BOUND('',#1855,.T.);
#749=FACE_BOUND('',#1863,.T.);
#750=FACE_BOUND('',#1866,.T.);
#751=FACE_BOUND('',#1868,.T.);
#752=FACE_BOUND('',#1874,.T.);
#753=FACE_BOUND('',#1877,.T.);
#754=FACE_BOUND('',#1879,.T.);
#755=FACE_BOUND('',#1880,.T.);
#756=FACE_BOUND('',#1888,.T.);
#757=FACE_BOUND('',#1891,.T.);
#758=FACE_BOUND('',#1893,.T.);
#759=FACE_BOUND('',#1899,.T.);
#760=FACE_BOUND('',#1902,.T.);
#761=FACE_BOUND('',#1904,.T.);
#762=FACE_BOUND('',#1905,.T.);
#763=FACE_BOUND('',#1913,.T.);
#764=FACE_BOUND('',#1916,.T.);
#765=FACE_BOUND('',#1918,.T.);
#766=FACE_BOUND('',#1924,.T.);
#767=FACE_BOUND('',#1927,.T.);
#768=FACE_BOUND('',#1929,.T.);
#769=FACE_BOUND('',#1930,.T.);
#770=FACE_BOUND('',#1939,.T.);
#771=FACE_BOUND('',#1941,.T.);
#772=FACE_BOUND('',#1946,.T.);
#773=FACE_BOUND('',#1947,.T.);
#774=FACE_BOUND('',#1948,.T.);
#775=FACE_BOUND('',#1949,.T.);
#776=FACE_BOUND('',#1950,.T.);
#777=FACE_BOUND('',#1953,.T.);
#778=FACE_BOUND('',#1954,.T.);
#779=FACE_BOUND('',#1955,.T.);
#780=FACE_BOUND('',#1956,.T.);
#781=FACE_BOUND('',#1957,.T.);
#782=FACE_BOUND('',#1960,.T.);
#783=FACE_BOUND('',#1961,.T.);
#784=FACE_BOUND('',#1968,.T.);
#785=FACE_BOUND('',#1972,.T.);
#786=FACE_BOUND('',#1973,.T.);
#787=FACE_BOUND('',#1974,.T.);
#788=FACE_BOUND('',#1975,.T.);
#789=FACE_BOUND('',#1976,.T.);
#790=FACE_BOUND('',#1978,.T.);
#791=FACE_BOUND('',#1979,.T.);
#792=FACE_BOUND('',#1980,.T.);
#793=FACE_BOUND('',#1981,.T.);
#794=FACE_BOUND('',#1982,.T.);
#795=FACE_BOUND('',#1989,.T.);
#796=FACE_BOUND('',#1993,.T.);
#797=FACE_BOUND('',#1994,.T.);
#798=FACE_BOUND('',#1995,.T.);
#799=FACE_BOUND('',#1996,.T.);
#800=FACE_BOUND('',#1997,.T.);
#801=FACE_BOUND('',#1999,.T.);
#802=FACE_BOUND('',#2000,.T.);
#803=FACE_BOUND('',#2001,.T.);
#804=FACE_BOUND('',#2002,.T.);
#805=FACE_BOUND('',#2003,.T.);
#806=FACE_BOUND('',#2012,.T.);
#807=FACE_BOUND('',#2014,.T.);
#808=FACE_BOUND('',#2019,.T.);
#809=FACE_BOUND('',#2020,.T.);
#810=FACE_BOUND('',#2021,.T.);
#811=FACE_BOUND('',#2022,.T.);
#812=FACE_BOUND('',#2023,.T.);
#813=FACE_BOUND('',#2026,.T.);
#814=FACE_BOUND('',#2027,.T.);
#815=FACE_BOUND('',#2028,.T.);
#816=FACE_BOUND('',#2029,.T.);
#817=FACE_BOUND('',#2030,.T.);
#818=FACE_BOUND('',#2033,.T.);
#819=FACE_BOUND('',#2034,.T.);
#820=FACE_BOUND('',#2041,.T.);
#821=FACE_BOUND('',#2045,.T.);
#822=FACE_BOUND('',#2046,.T.);
#823=FACE_BOUND('',#2047,.T.);
#824=FACE_BOUND('',#2048,.T.);
#825=FACE_BOUND('',#2049,.T.);
#826=FACE_BOUND('',#2051,.T.);
#827=FACE_BOUND('',#2052,.T.);
#828=FACE_BOUND('',#2053,.T.);
#829=FACE_BOUND('',#2054,.T.);
#830=FACE_BOUND('',#2055,.T.);
#831=FACE_BOUND('',#2062,.T.);
#832=FACE_BOUND('',#2066,.T.);
#833=FACE_BOUND('',#2067,.T.);
#834=FACE_BOUND('',#2068,.T.);
#835=FACE_BOUND('',#2069,.T.);
#836=FACE_BOUND('',#2070,.T.);
#837=FACE_BOUND('',#2072,.T.);
#838=FACE_BOUND('',#2073,.T.);
#839=FACE_BOUND('',#2074,.T.);
#840=FACE_BOUND('',#2075,.T.);
#841=FACE_BOUND('',#2076,.T.);
#842=FACE_BOUND('',#2087,.T.);
#843=FACE_BOUND('',#2090,.T.);
#844=FACE_BOUND('',#2095,.T.);
#845=FACE_BOUND('',#2100,.T.);
#846=FACE_BOUND('',#2125,.T.);
#847=FACE_BOUND('',#2128,.T.);
#848=FACE_BOUND('',#2131,.T.);
#849=FACE_BOUND('',#2134,.T.);
#850=FACE_BOUND('',#2137,.T.);
#851=FACE_BOUND('',#2160,.T.);
#852=FACE_BOUND('',#2161,.T.);
#853=FACE_BOUND('',#2162,.T.);
#854=FACE_BOUND('',#2163,.T.);
#855=FACE_BOUND('',#2164,.T.);
#856=FACE_BOUND('',#2165,.T.);
#857=FACE_BOUND('',#2166,.T.);
#858=FACE_BOUND('',#2167,.T.);
#859=FACE_BOUND('',#2168,.T.);
#860=FACE_BOUND('',#2169,.T.);
#861=FACE_BOUND('',#2170,.T.);
#862=FACE_BOUND('',#2171,.T.);
#863=FACE_BOUND('',#2172,.T.);
#864=FACE_BOUND('',#2175,.T.);
#865=FACE_BOUND('',#2176,.T.);
#866=FACE_BOUND('',#2177,.T.);
#867=FACE_BOUND('',#2178,.T.);
#868=FACE_BOUND('',#2179,.T.);
#869=FACE_BOUND('',#2180,.T.);
#870=FACE_BOUND('',#2181,.T.);
#871=FACE_BOUND('',#2193,.T.);
#872=FACE_BOUND('',#2194,.T.);
#873=FACE_BOUND('',#2195,.T.);
#874=FACE_BOUND('',#2196,.T.);
#875=FACE_BOUND('',#2197,.T.);
#876=FACE_BOUND('',#2198,.T.);
#877=FACE_BOUND('',#2199,.T.);
#878=FACE_BOUND('',#2202,.T.);
#879=FACE_BOUND('',#2203,.T.);
#880=FACE_BOUND('',#2204,.T.);
#881=FACE_BOUND('',#2205,.T.);
#882=FACE_BOUND('',#2206,.T.);
#883=FACE_BOUND('',#2207,.T.);
#884=FACE_BOUND('',#2208,.T.);
#885=FACE_BOUND('',#2220,.T.);
#886=FACE_BOUND('',#2221,.T.);
#887=FACE_BOUND('',#2222,.T.);
#888=FACE_BOUND('',#2223,.T.);
#889=FACE_BOUND('',#2224,.T.);
#890=FACE_BOUND('',#2225,.T.);
#891=FACE_BOUND('',#2226,.T.);
#892=FACE_BOUND('',#2229,.T.);
#893=FACE_BOUND('',#2230,.T.);
#894=FACE_BOUND('',#2231,.T.);
#895=FACE_BOUND('',#2232,.T.);
#896=FACE_BOUND('',#2233,.T.);
#897=FACE_BOUND('',#2234,.T.);
#898=FACE_BOUND('',#2235,.T.);
#899=FACE_BOUND('',#2244,.T.);
#900=FACE_BOUND('',#2247,.T.);
#901=FACE_BOUND('',#2248,.T.);
#902=FACE_BOUND('',#2249,.T.);
#903=FACE_BOUND('',#2252,.T.);
#904=FACE_BOUND('',#2255,.T.);
#905=FACE_BOUND('',#2258,.T.);
#906=FACE_BOUND('',#2261,.T.);
#907=FACE_BOUND('',#2264,.T.);
#908=FACE_BOUND('',#2271,.T.);
#909=FACE_BOUND('',#2272,.T.);
#910=FACE_BOUND('',#2273,.T.);
#911=FACE_BOUND('',#2274,.T.);
#912=FACE_BOUND('',#2277,.T.);
#913=FACE_BOUND('',#2278,.T.);
#914=FACE_BOUND('',#2279,.T.);
#915=FACE_BOUND('',#2280,.T.);
#916=FACE_BOUND('',#2304,.T.);
#917=FACE_BOUND('',#2305,.T.);
#918=FACE_BOUND('',#2306,.T.);
#919=FACE_BOUND('',#2307,.T.);
#920=FACE_BOUND('',#2308,.T.);
#921=FACE_BOUND('',#2309,.T.);
#922=FACE_BOUND('',#2310,.T.);
#923=FACE_BOUND('',#2313,.T.);
#924=FACE_BOUND('',#2314,.T.);
#925=FACE_BOUND('',#2315,.T.);
#926=FACE_BOUND('',#2316,.T.);
#927=FACE_BOUND('',#2317,.T.);
#928=FACE_BOUND('',#2318,.T.);
#929=FACE_BOUND('',#2319,.T.);
#930=FACE_BOUND('',#2320,.T.);
#931=FACE_BOUND('',#2321,.T.);
#932=FACE_BOUND('',#2322,.T.);
#933=FACE_BOUND('',#2323,.T.);
#934=FACE_BOUND('',#2324,.T.);
#935=FACE_BOUND('',#2325,.T.);
#936=FACE_BOUND('',#2337,.T.);
#937=FACE_BOUND('',#2338,.T.);
#938=FACE_BOUND('',#2339,.T.);
#939=FACE_BOUND('',#2340,.T.);
#940=FACE_BOUND('',#2341,.T.);
#941=FACE_BOUND('',#2342,.T.);
#942=FACE_BOUND('',#2343,.T.);
#943=FACE_BOUND('',#2346,.T.);
#944=FACE_BOUND('',#2347,.T.);
#945=FACE_BOUND('',#2348,.T.);
#946=FACE_BOUND('',#2349,.T.);
#947=FACE_BOUND('',#2350,.T.);
#948=FACE_BOUND('',#2351,.T.);
#949=FACE_BOUND('',#2352,.T.);
#950=FACE_BOUND('',#2364,.T.);
#951=FACE_BOUND('',#2365,.T.);
#952=FACE_BOUND('',#2366,.T.);
#953=FACE_BOUND('',#2367,.T.);
#954=FACE_BOUND('',#2368,.T.);
#955=FACE_BOUND('',#2369,.T.);
#956=FACE_BOUND('',#2370,.T.);
#957=FACE_BOUND('',#2373,.T.);
#958=FACE_BOUND('',#2374,.T.);
#959=FACE_BOUND('',#2375,.T.);
#960=FACE_BOUND('',#2376,.T.);
#961=FACE_BOUND('',#2377,.T.);
#962=FACE_BOUND('',#2378,.T.);
#963=FACE_BOUND('',#2379,.T.);
#964=FACE_BOUND('',#2388,.T.);
#965=FACE_BOUND('',#2391,.T.);
#966=FACE_BOUND('',#2392,.T.);
#967=FACE_BOUND('',#2393,.T.);
#968=FACE_BOUND('',#2396,.T.);
#969=FACE_BOUND('',#2399,.T.);
#970=FACE_BOUND('',#2402,.T.);
#971=FACE_BOUND('',#2405,.T.);
#972=FACE_BOUND('',#2408,.T.);
#973=FACE_BOUND('',#2415,.T.);
#974=FACE_BOUND('',#2416,.T.);
#975=FACE_BOUND('',#2417,.T.);
#976=FACE_BOUND('',#2418,.T.);
#977=FACE_BOUND('',#2421,.T.);
#978=FACE_BOUND('',#2422,.T.);
#979=FACE_BOUND('',#2423,.T.);
#980=FACE_BOUND('',#2424,.T.);
#981=FACE_BOUND('',#2433,.T.);
#982=FACE_BOUND('',#2436,.T.);
#983=FACE_BOUND('',#2439,.T.);
#984=FACE_BOUND('',#2442,.T.);
#985=FACE_BOUND('',#2445,.T.);
#986=FACE_BOUND('',#2448,.T.);
#987=FACE_BOUND('',#2450,.T.);
#988=FACE_BOUND('',#2456,.T.);
#989=FACE_BOUND('',#2458,.T.);
#990=FACE_BOUND('',#2460,.T.);
#991=FACE_BOUND('',#2462,.T.);
#992=FACE_BOUND('',#2477,.T.);
#993=FACE_BOUND('',#2485,.T.);
#994=FACE_BOUND('',#2487,.T.);
#995=FACE_BOUND('',#2491,.T.);
#996=FACE_BOUND('',#2493,.T.);
#997=FACE_BOUND('',#2498,.T.);
#998=FACE_BOUND('',#2500,.T.);
#999=FACE_BOUND('',#2504,.T.);
#1000=FACE_BOUND('',#2506,.T.);
#1001=FACE_BOUND('',#2510,.T.);
#1002=FACE_BOUND('',#2512,.T.);
#1003=FACE_BOUND('',#2518,.T.);
#1004=FACE_BOUND('',#2522,.T.);
#1005=FACE_BOUND('',#2524,.T.);
#1006=FACE_BOUND('',#2528,.T.);
#1007=FACE_BOUND('',#2530,.T.);
#1008=FACE_BOUND('',#2534,.T.);
#1009=FACE_BOUND('',#2536,.T.);
#1010=FACE_BOUND('',#2543,.T.);
#1011=FACE_BOUND('',#2545,.T.);
#1012=FACE_BOUND('',#2551,.T.);
#1013=FACE_BOUND('',#2572,.T.);
#1014=PLANE('',#9616);
#1015=PLANE('',#9617);
#1016=PLANE('',#9618);
#1017=PLANE('',#9619);
#1018=PLANE('',#9620);
#1019=PLANE('',#9621);
#1020=PLANE('',#9623);
#1021=PLANE('',#9624);
#1022=PLANE('',#9625);
#1023=PLANE('',#9626);
#1024=PLANE('',#9627);
#1025=PLANE('',#9628);
#1026=PLANE('',#9630);
#1027=PLANE('',#9631);
#1028=PLANE('',#9632);
#1029=PLANE('',#9633);
#1030=PLANE('',#9634);
#1031=PLANE('',#9635);
#1032=PLANE('',#9643);
#1033=PLANE('',#9648);
#1034=PLANE('',#9652);
#1035=PLANE('',#9657);
#1036=PLANE('',#9659);
#1037=PLANE('',#9667);
#1038=PLANE('',#9668);
#1039=PLANE('',#9669);
#1040=PLANE('',#9670);
#1041=PLANE('',#9671);
#1042=PLANE('',#9679);
#1043=PLANE('',#9684);
#1044=PLANE('',#9688);
#1045=PLANE('',#9693);
#1046=PLANE('',#9695);
#1047=PLANE('',#9703);
#1048=PLANE('',#9704);
#1049=PLANE('',#9705);
#1050=PLANE('',#9706);
#1051=PLANE('',#9707);
#1052=PLANE('',#9715);
#1053=PLANE('',#9720);
#1054=PLANE('',#9724);
#1055=PLANE('',#9729);
#1056=PLANE('',#9731);
#1057=PLANE('',#9739);
#1058=PLANE('',#9740);
#1059=PLANE('',#9741);
#1060=PLANE('',#9742);
#1061=PLANE('',#9743);
#1062=PLANE('',#9751);
#1063=PLANE('',#9756);
#1064=PLANE('',#9760);
#1065=PLANE('',#9765);
#1066=PLANE('',#9767);
#1067=PLANE('',#9775);
#1068=PLANE('',#9776);
#1069=PLANE('',#9777);
#1070=PLANE('',#9778);
#1071=PLANE('',#9779);
#1072=PLANE('',#9802);
#1073=PLANE('',#9803);
#1074=PLANE('',#9804);
#1075=PLANE('',#9805);
#1076=PLANE('',#9806);
#1077=PLANE('',#9807);
#1078=PLANE('',#9808);
#1079=PLANE('',#9809);
#1080=PLANE('',#9810);
#1081=PLANE('',#9811);
#1082=PLANE('',#9828);
#1083=PLANE('',#9835);
#1084=PLANE('',#9836);
#1085=PLANE('',#9853);
#1086=PLANE('',#9860);
#1087=PLANE('',#9861);
#1088=PLANE('',#9884);
#1089=PLANE('',#9885);
#1090=PLANE('',#9886);
#1091=PLANE('',#9887);
#1092=PLANE('',#9888);
#1093=PLANE('',#9889);
#1094=PLANE('',#9890);
#1095=PLANE('',#9891);
#1096=PLANE('',#9892);
#1097=PLANE('',#9893);
#1098=PLANE('',#9910);
#1099=PLANE('',#9917);
#1100=PLANE('',#9918);
#1101=PLANE('',#9935);
#1102=PLANE('',#9942);
#1103=PLANE('',#9943);
#1104=PLANE('',#9950);
#1105=PLANE('',#9953);
#1106=PLANE('',#9969);
#1107=PLANE('',#9972);
#1108=PLANE('',#9984);
#1109=PLANE('',#9993);
#1110=PLANE('',#10024);
#1111=PLANE('',#10029);
#1112=PLANE('',#10034);
#1113=PLANE('',#10040);
#1114=PLANE('',#10045);
#1115=PLANE('',#10054);
#1116=PLANE('',#10058);
#1117=PLANE('',#10059);
#1118=PLANE('',#10061);
#1119=PLANE('',#10066);
#1120=PLANE('',#10069);
#1121=PLANE('',#10074);
#1122=PLANE('',#10087);
#1123=PLANE('',#10091);
#1124=PLANE('',#10095);
#1125=PLANE('',#10099);
#1126=PLANE('',#10103);
#1127=PLANE('',#10107);
#1128=PLANE('',#10129);
#1129=PLANE('',#10130);
#1130=PLANE('',#10131);
#1131=PLANE('',#10132);
#1132=PLANE('',#10133);
#1133=PLANE('',#10134);
#1134=PLANE('',#10157);
#1135=PLANE('',#10158);
#1136=PLANE('',#10159);
#1137=PLANE('',#10160);
#1138=PLANE('',#10161);
#1139=PLANE('',#10162);
#1140=PLANE('',#10185);
#1141=PLANE('',#10186);
#1142=PLANE('',#10187);
#1143=PLANE('',#10188);
#1144=PLANE('',#10189);
#1145=PLANE('',#10190);
#1146=PLANE('',#10192);
#1147=PLANE('',#10199);
#1148=PLANE('',#10211);
#1149=PLANE('',#10215);
#1150=PLANE('',#10219);
#1151=PLANE('',#10224);
#1152=PLANE('',#10229);
#1153=PLANE('',#10234);
#1154=PLANE('',#10239);
#1155=PLANE('',#10249);
#1156=PLANE('',#10250);
#1157=PLANE('',#10251);
#1158=PLANE('',#10252);
#1159=PLANE('',#10253);
#1160=PLANE('',#10254);
#1161=PLANE('',#10260);
#1162=PLANE('',#10264);
#1163=PLANE('',#10268);
#1164=PLANE('',#10272);
#1165=PLANE('',#10276);
#1166=PLANE('',#10280);
#1167=PLANE('',#10302);
#1168=PLANE('',#10303);
#1169=PLANE('',#10304);
#1170=PLANE('',#10305);
#1171=PLANE('',#10306);
#1172=PLANE('',#10307);
#1173=PLANE('',#10330);
#1174=PLANE('',#10331);
#1175=PLANE('',#10332);
#1176=PLANE('',#10333);
#1177=PLANE('',#10334);
#1178=PLANE('',#10335);
#1179=PLANE('',#10358);
#1180=PLANE('',#10359);
#1181=PLANE('',#10360);
#1182=PLANE('',#10361);
#1183=PLANE('',#10362);
#1184=PLANE('',#10363);
#1185=PLANE('',#10365);
#1186=PLANE('',#10372);
#1187=PLANE('',#10384);
#1188=PLANE('',#10388);
#1189=PLANE('',#10392);
#1190=PLANE('',#10397);
#1191=PLANE('',#10402);
#1192=PLANE('',#10407);
#1193=PLANE('',#10412);
#1194=PLANE('',#10422);
#1195=PLANE('',#10423);
#1196=PLANE('',#10424);
#1197=PLANE('',#10425);
#1198=PLANE('',#10426);
#1199=PLANE('',#10427);
#1200=PLANE('',#10430);
#1201=PLANE('',#10432);
#1202=PLANE('',#10433);
#1203=PLANE('',#10435);
#1204=PLANE('',#10436);
#1205=PLANE('',#10437);
#1206=PLANE('',#10442);
#1207=PLANE('',#10446);
#1208=PLANE('',#10450);
#1209=PLANE('',#10454);
#1210=PLANE('',#10458);
#1211=PLANE('',#10462);
#1212=PLANE('',#10465);
#1213=PLANE('',#10466);
#1214=PLANE('',#10469);
#1215=PLANE('',#10470);
#1216=PLANE('',#10475);
#1217=PLANE('',#10481);
#1218=PLANE('',#10482);
#1219=PLANE('',#10483);
#1220=PLANE('',#10484);
#1221=PLANE('',#10485);
#1222=PLANE('',#10486);
#1223=PLANE('',#10487);
#1224=PLANE('',#10488);
#1225=PLANE('',#10489);
#1226=PLANE('',#10491);
#1227=PLANE('',#10499);
#1228=PLANE('',#10509);
#1229=PLANE('',#10513);
#1230=PLANE('',#10514);
#1231=PLANE('',#10517);
#1232=PLANE('',#10523);
#1233=PLANE('',#10525);
#1234=PLANE('',#10533);
#1235=PLANE('',#10534);
#1236=PLANE('',#10542);
#1237=PLANE('',#10543);
#1238=PLANE('',#10551);
#1239=PLANE('',#10552);
#1240=PLANE('',#10557);
#1241=PLANE('',#10561);
#1242=PLANE('',#10562);
#1243=PLANE('',#10569);
#1244=PLANE('',#10570);
#1245=PLANE('',#10578);
#1246=PLANE('',#10579);
#1247=PLANE('',#10587);
#1248=PLANE('',#10588);
#1249=PLANE('',#10590);
#1250=PLANE('',#10594);
#1251=PLANE('',#10601);
#1252=PLANE('',#10602);
#1253=PLANE('',#10604);
#1254=PLANE('',#10612);
#1255=PLANE('',#10620);
#1256=PLANE('',#10621);
#1257=PLANE('',#10622);
#1258=PLANE('',#10623);
#1259=PLANE('',#10624);
#1260=PLANE('',#10625);
#1261=PLANE('',#10626);
#1262=PLANE('',#10627);
#1263=PLANE('',#10628);
#1264=PLANE('',#10672);
#1265=PLANE('',#10673);
#1266=PLANE('',#10674);
#1267=PLANE('',#10675);
#1268=PLANE('',#10676);
#1269=PLANE('',#10677);
#1270=PLANE('',#10678);
#1271=PLANE('',#10679);
#1272=PLANE('',#10687);
#1273=FACE_OUTER_BOUND('',#1777,.T.);
#1274=FACE_OUTER_BOUND('',#1778,.T.);
#1275=FACE_OUTER_BOUND('',#1779,.T.);
#1276=FACE_OUTER_BOUND('',#1780,.T.);
#1277=FACE_OUTER_BOUND('',#1781,.T.);
#1278=FACE_OUTER_BOUND('',#1782,.T.);
#1279=FACE_OUTER_BOUND('',#1783,.T.);
#1280=FACE_OUTER_BOUND('',#1784,.T.);
#1281=FACE_OUTER_BOUND('',#1785,.T.);
#1282=FACE_OUTER_BOUND('',#1786,.T.);
#1283=FACE_OUTER_BOUND('',#1787,.T.);
#1284=FACE_OUTER_BOUND('',#1788,.T.);
#1285=FACE_OUTER_BOUND('',#1789,.T.);
#1286=FACE_OUTER_BOUND('',#1790,.T.);
#1287=FACE_OUTER_BOUND('',#1791,.T.);
#1288=FACE_OUTER_BOUND('',#1792,.T.);
#1289=FACE_OUTER_BOUND('',#1793,.T.);
#1290=FACE_OUTER_BOUND('',#1806,.T.);
#1291=FACE_OUTER_BOUND('',#1819,.T.);
#1292=FACE_OUTER_BOUND('',#1820,.T.);
#1293=FACE_OUTER_BOUND('',#1821,.T.);
#1294=FACE_OUTER_BOUND('',#1822,.T.);
#1295=FACE_OUTER_BOUND('',#1823,.T.);
#1296=FACE_OUTER_BOUND('',#1824,.T.);
#1297=FACE_OUTER_BOUND('',#1825,.T.);
#1298=FACE_OUTER_BOUND('',#1826,.T.);
#1299=FACE_OUTER_BOUND('',#1827,.T.);
#1300=FACE_OUTER_BOUND('',#1828,.T.);
#1301=FACE_OUTER_BOUND('',#1829,.T.);
#1302=FACE_OUTER_BOUND('',#1830,.T.);
#1303=FACE_OUTER_BOUND('',#1831,.T.);
#1304=FACE_OUTER_BOUND('',#1832,.T.);
#1305=FACE_OUTER_BOUND('',#1833,.T.);
#1306=FACE_OUTER_BOUND('',#1834,.T.);
#1307=FACE_OUTER_BOUND('',#1835,.T.);
#1308=FACE_OUTER_BOUND('',#1836,.T.);
#1309=FACE_OUTER_BOUND('',#1837,.T.);
#1310=FACE_OUTER_BOUND('',#1839,.T.);
#1311=FACE_OUTER_BOUND('',#1840,.T.);
#1312=FACE_OUTER_BOUND('',#1842,.T.);
#1313=FACE_OUTER_BOUND('',#1844,.T.);
#1314=FACE_OUTER_BOUND('',#1845,.T.);
#1315=FACE_OUTER_BOUND('',#1846,.T.);
#1316=FACE_OUTER_BOUND('',#1847,.T.);
#1317=FACE_OUTER_BOUND('',#1848,.T.);
#1318=FACE_OUTER_BOUND('',#1850,.T.);
#1319=FACE_OUTER_BOUND('',#1851,.T.);
#1320=FACE_OUTER_BOUND('',#1853,.T.);
#1321=FACE_OUTER_BOUND('',#1856,.T.);
#1322=FACE_OUTER_BOUND('',#1857,.T.);
#1323=FACE_OUTER_BOUND('',#1858,.T.);
#1324=FACE_OUTER_BOUND('',#1859,.T.);
#1325=FACE_OUTER_BOUND('',#1860,.T.);
#1326=FACE_OUTER_BOUND('',#1861,.T.);
#1327=FACE_OUTER_BOUND('',#1862,.T.);
#1328=FACE_OUTER_BOUND('',#1864,.T.);
#1329=FACE_OUTER_BOUND('',#1865,.T.);
#1330=FACE_OUTER_BOUND('',#1867,.T.);
#1331=FACE_OUTER_BOUND('',#1869,.T.);
#1332=FACE_OUTER_BOUND('',#1870,.T.);
#1333=FACE_OUTER_BOUND('',#1871,.T.);
#1334=FACE_OUTER_BOUND('',#1872,.T.);
#1335=FACE_OUTER_BOUND('',#1873,.T.);
#1336=FACE_OUTER_BOUND('',#1875,.T.);
#1337=FACE_OUTER_BOUND('',#1876,.T.);
#1338=FACE_OUTER_BOUND('',#1878,.T.);
#1339=FACE_OUTER_BOUND('',#1881,.T.);
#1340=FACE_OUTER_BOUND('',#1882,.T.);
#1341=FACE_OUTER_BOUND('',#1883,.T.);
#1342=FACE_OUTER_BOUND('',#1884,.T.);
#1343=FACE_OUTER_BOUND('',#1885,.T.);
#1344=FACE_OUTER_BOUND('',#1886,.T.);
#1345=FACE_OUTER_BOUND('',#1887,.T.);
#1346=FACE_OUTER_BOUND('',#1889,.T.);
#1347=FACE_OUTER_BOUND('',#1890,.T.);
#1348=FACE_OUTER_BOUND('',#1892,.T.);
#1349=FACE_OUTER_BOUND('',#1894,.T.);
#1350=FACE_OUTER_BOUND('',#1895,.T.);
#1351=FACE_OUTER_BOUND('',#1896,.T.);
#1352=FACE_OUTER_BOUND('',#1897,.T.);
#1353=FACE_OUTER_BOUND('',#1898,.T.);
#1354=FACE_OUTER_BOUND('',#1900,.T.);
#1355=FACE_OUTER_BOUND('',#1901,.T.);
#1356=FACE_OUTER_BOUND('',#1903,.T.);
#1357=FACE_OUTER_BOUND('',#1906,.T.);
#1358=FACE_OUTER_BOUND('',#1907,.T.);
#1359=FACE_OUTER_BOUND('',#1908,.T.);
#1360=FACE_OUTER_BOUND('',#1909,.T.);
#1361=FACE_OUTER_BOUND('',#1910,.T.);
#1362=FACE_OUTER_BOUND('',#1911,.T.);
#1363=FACE_OUTER_BOUND('',#1912,.T.);
#1364=FACE_OUTER_BOUND('',#1914,.T.);
#1365=FACE_OUTER_BOUND('',#1915,.T.);
#1366=FACE_OUTER_BOUND('',#1917,.T.);
#1367=FACE_OUTER_BOUND('',#1919,.T.);
#1368=FACE_OUTER_BOUND('',#1920,.T.);
#1369=FACE_OUTER_BOUND('',#1921,.T.);
#1370=FACE_OUTER_BOUND('',#1922,.T.);
#1371=FACE_OUTER_BOUND('',#1923,.T.);
#1372=FACE_OUTER_BOUND('',#1925,.T.);
#1373=FACE_OUTER_BOUND('',#1926,.T.);
#1374=FACE_OUTER_BOUND('',#1928,.T.);
#1375=FACE_OUTER_BOUND('',#1931,.T.);
#1376=FACE_OUTER_BOUND('',#1932,.T.);
#1377=FACE_OUTER_BOUND('',#1933,.T.);
#1378=FACE_OUTER_BOUND('',#1934,.T.);
#1379=FACE_OUTER_BOUND('',#1935,.T.);
#1380=FACE_OUTER_BOUND('',#1936,.T.);
#1381=FACE_OUTER_BOUND('',#1937,.T.);
#1382=FACE_OUTER_BOUND('',#1938,.T.);
#1383=FACE_OUTER_BOUND('',#1940,.T.);
#1384=FACE_OUTER_BOUND('',#1942,.T.);
#1385=FACE_OUTER_BOUND('',#1943,.T.);
#1386=FACE_OUTER_BOUND('',#1944,.T.);
#1387=FACE_OUTER_BOUND('',#1945,.T.);
#1388=FACE_OUTER_BOUND('',#1951,.T.);
#1389=FACE_OUTER_BOUND('',#1952,.T.);
#1390=FACE_OUTER_BOUND('',#1958,.T.);
#1391=FACE_OUTER_BOUND('',#1959,.T.);
#1392=FACE_OUTER_BOUND('',#1962,.T.);
#1393=FACE_OUTER_BOUND('',#1963,.T.);
#1394=FACE_OUTER_BOUND('',#1964,.T.);
#1395=FACE_OUTER_BOUND('',#1965,.T.);
#1396=FACE_OUTER_BOUND('',#1966,.T.);
#1397=FACE_OUTER_BOUND('',#1967,.T.);
#1398=FACE_OUTER_BOUND('',#1969,.T.);
#1399=FACE_OUTER_BOUND('',#1970,.T.);
#1400=FACE_OUTER_BOUND('',#1971,.T.);
#1401=FACE_OUTER_BOUND('',#1977,.T.);
#1402=FACE_OUTER_BOUND('',#1983,.T.);
#1403=FACE_OUTER_BOUND('',#1984,.T.);
#1404=FACE_OUTER_BOUND('',#1985,.T.);
#1405=FACE_OUTER_BOUND('',#1986,.T.);
#1406=FACE_OUTER_BOUND('',#1987,.T.);
#1407=FACE_OUTER_BOUND('',#1988,.T.);
#1408=FACE_OUTER_BOUND('',#1990,.T.);
#1409=FACE_OUTER_BOUND('',#1991,.T.);
#1410=FACE_OUTER_BOUND('',#1992,.T.);
#1411=FACE_OUTER_BOUND('',#1998,.T.);
#1412=FACE_OUTER_BOUND('',#2004,.T.);
#1413=FACE_OUTER_BOUND('',#2005,.T.);
#1414=FACE_OUTER_BOUND('',#2006,.T.);
#1415=FACE_OUTER_BOUND('',#2007,.T.);
#1416=FACE_OUTER_BOUND('',#2008,.T.);
#1417=FACE_OUTER_BOUND('',#2009,.T.);
#1418=FACE_OUTER_BOUND('',#2010,.T.);
#1419=FACE_OUTER_BOUND('',#2011,.T.);
#1420=FACE_OUTER_BOUND('',#2013,.T.);
#1421=FACE_OUTER_BOUND('',#2015,.T.);
#1422=FACE_OUTER_BOUND('',#2016,.T.);
#1423=FACE_OUTER_BOUND('',#2017,.T.);
#1424=FACE_OUTER_BOUND('',#2018,.T.);
#1425=FACE_OUTER_BOUND('',#2024,.T.);
#1426=FACE_OUTER_BOUND('',#2025,.T.);
#1427=FACE_OUTER_BOUND('',#2031,.T.);
#1428=FACE_OUTER_BOUND('',#2032,.T.);
#1429=FACE_OUTER_BOUND('',#2035,.T.);
#1430=FACE_OUTER_BOUND('',#2036,.T.);
#1431=FACE_OUTER_BOUND('',#2037,.T.);
#1432=FACE_OUTER_BOUND('',#2038,.T.);
#1433=FACE_OUTER_BOUND('',#2039,.T.);
#1434=FACE_OUTER_BOUND('',#2040,.T.);
#1435=FACE_OUTER_BOUND('',#2042,.T.);
#1436=FACE_OUTER_BOUND('',#2043,.T.);
#1437=FACE_OUTER_BOUND('',#2044,.T.);
#1438=FACE_OUTER_BOUND('',#2050,.T.);
#1439=FACE_OUTER_BOUND('',#2056,.T.);
#1440=FACE_OUTER_BOUND('',#2057,.T.);
#1441=FACE_OUTER_BOUND('',#2058,.T.);
#1442=FACE_OUTER_BOUND('',#2059,.T.);
#1443=FACE_OUTER_BOUND('',#2060,.T.);
#1444=FACE_OUTER_BOUND('',#2061,.T.);
#1445=FACE_OUTER_BOUND('',#2063,.T.);
#1446=FACE_OUTER_BOUND('',#2064,.T.);
#1447=FACE_OUTER_BOUND('',#2065,.T.);
#1448=FACE_OUTER_BOUND('',#2071,.T.);
#1449=FACE_OUTER_BOUND('',#2077,.T.);
#1450=FACE_OUTER_BOUND('',#2078,.T.);
#1451=FACE_OUTER_BOUND('',#2079,.T.);
#1452=FACE_OUTER_BOUND('',#2080,.T.);
#1453=FACE_OUTER_BOUND('',#2081,.T.);
#1454=FACE_OUTER_BOUND('',#2082,.T.);
#1455=FACE_OUTER_BOUND('',#2083,.T.);
#1456=FACE_OUTER_BOUND('',#2084,.T.);
#1457=FACE_OUTER_BOUND('',#2085,.T.);
#1458=FACE_OUTER_BOUND('',#2086,.T.);
#1459=FACE_OUTER_BOUND('',#2088,.T.);
#1460=FACE_OUTER_BOUND('',#2089,.T.);
#1461=FACE_OUTER_BOUND('',#2091,.T.);
#1462=FACE_OUTER_BOUND('',#2092,.T.);
#1463=FACE_OUTER_BOUND('',#2093,.T.);
#1464=FACE_OUTER_BOUND('',#2094,.T.);
#1465=FACE_OUTER_BOUND('',#2096,.T.);
#1466=FACE_OUTER_BOUND('',#2097,.T.);
#1467=FACE_OUTER_BOUND('',#2098,.T.);
#1468=FACE_OUTER_BOUND('',#2099,.T.);
#1469=FACE_OUTER_BOUND('',#2101,.T.);
#1470=FACE_OUTER_BOUND('',#2102,.T.);
#1471=FACE_OUTER_BOUND('',#2103,.T.);
#1472=FACE_OUTER_BOUND('',#2104,.T.);
#1473=FACE_OUTER_BOUND('',#2105,.T.);
#1474=FACE_OUTER_BOUND('',#2106,.T.);
#1475=FACE_OUTER_BOUND('',#2107,.T.);
#1476=FACE_OUTER_BOUND('',#2108,.T.);
#1477=FACE_OUTER_BOUND('',#2109,.T.);
#1478=FACE_OUTER_BOUND('',#2110,.T.);
#1479=FACE_OUTER_BOUND('',#2111,.T.);
#1480=FACE_OUTER_BOUND('',#2112,.T.);
#1481=FACE_OUTER_BOUND('',#2113,.T.);
#1482=FACE_OUTER_BOUND('',#2114,.T.);
#1483=FACE_OUTER_BOUND('',#2115,.T.);
#1484=FACE_OUTER_BOUND('',#2116,.T.);
#1485=FACE_OUTER_BOUND('',#2117,.T.);
#1486=FACE_OUTER_BOUND('',#2118,.T.);
#1487=FACE_OUTER_BOUND('',#2119,.T.);
#1488=FACE_OUTER_BOUND('',#2120,.T.);
#1489=FACE_OUTER_BOUND('',#2121,.T.);
#1490=FACE_OUTER_BOUND('',#2122,.T.);
#1491=FACE_OUTER_BOUND('',#2123,.T.);
#1492=FACE_OUTER_BOUND('',#2124,.T.);
#1493=FACE_OUTER_BOUND('',#2126,.T.);
#1494=FACE_OUTER_BOUND('',#2127,.T.);
#1495=FACE_OUTER_BOUND('',#2129,.T.);
#1496=FACE_OUTER_BOUND('',#2130,.T.);
#1497=FACE_OUTER_BOUND('',#2132,.T.);
#1498=FACE_OUTER_BOUND('',#2133,.T.);
#1499=FACE_OUTER_BOUND('',#2135,.T.);
#1500=FACE_OUTER_BOUND('',#2136,.T.);
#1501=FACE_OUTER_BOUND('',#2138,.T.);
#1502=FACE_OUTER_BOUND('',#2139,.T.);
#1503=FACE_OUTER_BOUND('',#2140,.T.);
#1504=FACE_OUTER_BOUND('',#2141,.T.);
#1505=FACE_OUTER_BOUND('',#2142,.T.);
#1506=FACE_OUTER_BOUND('',#2143,.T.);
#1507=FACE_OUTER_BOUND('',#2144,.T.);
#1508=FACE_OUTER_BOUND('',#2145,.T.);
#1509=FACE_OUTER_BOUND('',#2146,.T.);
#1510=FACE_OUTER_BOUND('',#2147,.T.);
#1511=FACE_OUTER_BOUND('',#2148,.T.);
#1512=FACE_OUTER_BOUND('',#2149,.T.);
#1513=FACE_OUTER_BOUND('',#2150,.T.);
#1514=FACE_OUTER_BOUND('',#2151,.T.);
#1515=FACE_OUTER_BOUND('',#2152,.T.);
#1516=FACE_OUTER_BOUND('',#2153,.T.);
#1517=FACE_OUTER_BOUND('',#2154,.T.);
#1518=FACE_OUTER_BOUND('',#2155,.T.);
#1519=FACE_OUTER_BOUND('',#2156,.T.);
#1520=FACE_OUTER_BOUND('',#2157,.T.);
#1521=FACE_OUTER_BOUND('',#2158,.T.);
#1522=FACE_OUTER_BOUND('',#2159,.T.);
#1523=FACE_OUTER_BOUND('',#2173,.T.);
#1524=FACE_OUTER_BOUND('',#2174,.T.);
#1525=FACE_OUTER_BOUND('',#2182,.T.);
#1526=FACE_OUTER_BOUND('',#2183,.T.);
#1527=FACE_OUTER_BOUND('',#2184,.T.);
#1528=FACE_OUTER_BOUND('',#2185,.T.);
#1529=FACE_OUTER_BOUND('',#2186,.T.);
#1530=FACE_OUTER_BOUND('',#2187,.T.);
#1531=FACE_OUTER_BOUND('',#2188,.T.);
#1532=FACE_OUTER_BOUND('',#2189,.T.);
#1533=FACE_OUTER_BOUND('',#2190,.T.);
#1534=FACE_OUTER_BOUND('',#2191,.T.);
#1535=FACE_OUTER_BOUND('',#2192,.T.);
#1536=FACE_OUTER_BOUND('',#2200,.T.);
#1537=FACE_OUTER_BOUND('',#2201,.T.);
#1538=FACE_OUTER_BOUND('',#2209,.T.);
#1539=FACE_OUTER_BOUND('',#2210,.T.);
#1540=FACE_OUTER_BOUND('',#2211,.T.);
#1541=FACE_OUTER_BOUND('',#2212,.T.);
#1542=FACE_OUTER_BOUND('',#2213,.T.);
#1543=FACE_OUTER_BOUND('',#2214,.T.);
#1544=FACE_OUTER_BOUND('',#2215,.T.);
#1545=FACE_OUTER_BOUND('',#2216,.T.);
#1546=FACE_OUTER_BOUND('',#2217,.T.);
#1547=FACE_OUTER_BOUND('',#2218,.T.);
#1548=FACE_OUTER_BOUND('',#2219,.T.);
#1549=FACE_OUTER_BOUND('',#2227,.T.);
#1550=FACE_OUTER_BOUND('',#2228,.T.);
#1551=FACE_OUTER_BOUND('',#2236,.T.);
#1552=FACE_OUTER_BOUND('',#2237,.T.);
#1553=FACE_OUTER_BOUND('',#2238,.T.);
#1554=FACE_OUTER_BOUND('',#2239,.T.);
#1555=FACE_OUTER_BOUND('',#2240,.T.);
#1556=FACE_OUTER_BOUND('',#2241,.T.);
#1557=FACE_OUTER_BOUND('',#2242,.T.);
#1558=FACE_OUTER_BOUND('',#2243,.T.);
#1559=FACE_OUTER_BOUND('',#2245,.T.);
#1560=FACE_OUTER_BOUND('',#2246,.T.);
#1561=FACE_OUTER_BOUND('',#2250,.T.);
#1562=FACE_OUTER_BOUND('',#2251,.T.);
#1563=FACE_OUTER_BOUND('',#2253,.T.);
#1564=FACE_OUTER_BOUND('',#2254,.T.);
#1565=FACE_OUTER_BOUND('',#2256,.T.);
#1566=FACE_OUTER_BOUND('',#2257,.T.);
#1567=FACE_OUTER_BOUND('',#2259,.T.);
#1568=FACE_OUTER_BOUND('',#2260,.T.);
#1569=FACE_OUTER_BOUND('',#2262,.T.);
#1570=FACE_OUTER_BOUND('',#2263,.T.);
#1571=FACE_OUTER_BOUND('',#2265,.T.);
#1572=FACE_OUTER_BOUND('',#2266,.T.);
#1573=FACE_OUTER_BOUND('',#2267,.T.);
#1574=FACE_OUTER_BOUND('',#2268,.T.);
#1575=FACE_OUTER_BOUND('',#2269,.T.);
#1576=FACE_OUTER_BOUND('',#2270,.T.);
#1577=FACE_OUTER_BOUND('',#2275,.T.);
#1578=FACE_OUTER_BOUND('',#2276,.T.);
#1579=FACE_OUTER_BOUND('',#2281,.T.);
#1580=FACE_OUTER_BOUND('',#2282,.T.);
#1581=FACE_OUTER_BOUND('',#2283,.T.);
#1582=FACE_OUTER_BOUND('',#2284,.T.);
#1583=FACE_OUTER_BOUND('',#2285,.T.);
#1584=FACE_OUTER_BOUND('',#2286,.T.);
#1585=FACE_OUTER_BOUND('',#2287,.T.);
#1586=FACE_OUTER_BOUND('',#2288,.T.);
#1587=FACE_OUTER_BOUND('',#2289,.T.);
#1588=FACE_OUTER_BOUND('',#2290,.T.);
#1589=FACE_OUTER_BOUND('',#2291,.T.);
#1590=FACE_OUTER_BOUND('',#2292,.T.);
#1591=FACE_OUTER_BOUND('',#2293,.T.);
#1592=FACE_OUTER_BOUND('',#2294,.T.);
#1593=FACE_OUTER_BOUND('',#2295,.T.);
#1594=FACE_OUTER_BOUND('',#2296,.T.);
#1595=FACE_OUTER_BOUND('',#2297,.T.);
#1596=FACE_OUTER_BOUND('',#2298,.T.);
#1597=FACE_OUTER_BOUND('',#2299,.T.);
#1598=FACE_OUTER_BOUND('',#2300,.T.);
#1599=FACE_OUTER_BOUND('',#2301,.T.);
#1600=FACE_OUTER_BOUND('',#2302,.T.);
#1601=FACE_OUTER_BOUND('',#2303,.T.);
#1602=FACE_OUTER_BOUND('',#2311,.T.);
#1603=FACE_OUTER_BOUND('',#2312,.T.);
#1604=FACE_OUTER_BOUND('',#2326,.T.);
#1605=FACE_OUTER_BOUND('',#2327,.T.);
#1606=FACE_OUTER_BOUND('',#2328,.T.);
#1607=FACE_OUTER_BOUND('',#2329,.T.);
#1608=FACE_OUTER_BOUND('',#2330,.T.);
#1609=FACE_OUTER_BOUND('',#2331,.T.);
#1610=FACE_OUTER_BOUND('',#2332,.T.);
#1611=FACE_OUTER_BOUND('',#2333,.T.);
#1612=FACE_OUTER_BOUND('',#2334,.T.);
#1613=FACE_OUTER_BOUND('',#2335,.T.);
#1614=FACE_OUTER_BOUND('',#2336,.T.);
#1615=FACE_OUTER_BOUND('',#2344,.T.);
#1616=FACE_OUTER_BOUND('',#2345,.T.);
#1617=FACE_OUTER_BOUND('',#2353,.T.);
#1618=FACE_OUTER_BOUND('',#2354,.T.);
#1619=FACE_OUTER_BOUND('',#2355,.T.);
#1620=FACE_OUTER_BOUND('',#2356,.T.);
#1621=FACE_OUTER_BOUND('',#2357,.T.);
#1622=FACE_OUTER_BOUND('',#2358,.T.);
#1623=FACE_OUTER_BOUND('',#2359,.T.);
#1624=FACE_OUTER_BOUND('',#2360,.T.);
#1625=FACE_OUTER_BOUND('',#2361,.T.);
#1626=FACE_OUTER_BOUND('',#2362,.T.);
#1627=FACE_OUTER_BOUND('',#2363,.T.);
#1628=FACE_OUTER_BOUND('',#2371,.T.);
#1629=FACE_OUTER_BOUND('',#2372,.T.);
#1630=FACE_OUTER_BOUND('',#2380,.T.);
#1631=FACE_OUTER_BOUND('',#2381,.T.);
#1632=FACE_OUTER_BOUND('',#2382,.T.);
#1633=FACE_OUTER_BOUND('',#2383,.T.);
#1634=FACE_OUTER_BOUND('',#2384,.T.);
#1635=FACE_OUTER_BOUND('',#2385,.T.);
#1636=FACE_OUTER_BOUND('',#2386,.T.);
#1637=FACE_OUTER_BOUND('',#2387,.T.);
#1638=FACE_OUTER_BOUND('',#2389,.T.);
#1639=FACE_OUTER_BOUND('',#2390,.T.);
#1640=FACE_OUTER_BOUND('',#2394,.T.);
#1641=FACE_OUTER_BOUND('',#2395,.T.);
#1642=FACE_OUTER_BOUND('',#2397,.T.);
#1643=FACE_OUTER_BOUND('',#2398,.T.);
#1644=FACE_OUTER_BOUND('',#2400,.T.);
#1645=FACE_OUTER_BOUND('',#2401,.T.);
#1646=FACE_OUTER_BOUND('',#2403,.T.);
#1647=FACE_OUTER_BOUND('',#2404,.T.);
#1648=FACE_OUTER_BOUND('',#2406,.T.);
#1649=FACE_OUTER_BOUND('',#2407,.T.);
#1650=FACE_OUTER_BOUND('',#2409,.T.);
#1651=FACE_OUTER_BOUND('',#2410,.T.);
#1652=FACE_OUTER_BOUND('',#2411,.T.);
#1653=FACE_OUTER_BOUND('',#2412,.T.);
#1654=FACE_OUTER_BOUND('',#2413,.T.);
#1655=FACE_OUTER_BOUND('',#2414,.T.);
#1656=FACE_OUTER_BOUND('',#2419,.T.);
#1657=FACE_OUTER_BOUND('',#2420,.T.);
#1658=FACE_OUTER_BOUND('',#2425,.T.);
#1659=FACE_OUTER_BOUND('',#2426,.T.);
#1660=FACE_OUTER_BOUND('',#2427,.T.);
#1661=FACE_OUTER_BOUND('',#2428,.T.);
#1662=FACE_OUTER_BOUND('',#2429,.T.);
#1663=FACE_OUTER_BOUND('',#2430,.T.);
#1664=FACE_OUTER_BOUND('',#2431,.T.);
#1665=FACE_OUTER_BOUND('',#2432,.T.);
#1666=FACE_OUTER_BOUND('',#2434,.T.);
#1667=FACE_OUTER_BOUND('',#2435,.T.);
#1668=FACE_OUTER_BOUND('',#2437,.T.);
#1669=FACE_OUTER_BOUND('',#2438,.T.);
#1670=FACE_OUTER_BOUND('',#2440,.T.);
#1671=FACE_OUTER_BOUND('',#2441,.T.);
#1672=FACE_OUTER_BOUND('',#2443,.T.);
#1673=FACE_OUTER_BOUND('',#2444,.T.);
#1674=FACE_OUTER_BOUND('',#2446,.T.);
#1675=FACE_OUTER_BOUND('',#2447,.T.);
#1676=FACE_OUTER_BOUND('',#2449,.T.);
#1677=FACE_OUTER_BOUND('',#2451,.T.);
#1678=FACE_OUTER_BOUND('',#2452,.T.);
#1679=FACE_OUTER_BOUND('',#2453,.T.);
#1680=FACE_OUTER_BOUND('',#2454,.T.);
#1681=FACE_OUTER_BOUND('',#2455,.T.);
#1682=FACE_OUTER_BOUND('',#2457,.T.);
#1683=FACE_OUTER_BOUND('',#2459,.T.);
#1684=FACE_OUTER_BOUND('',#2461,.T.);
#1685=FACE_OUTER_BOUND('',#2463,.T.);
#1686=FACE_OUTER_BOUND('',#2464,.T.);
#1687=FACE_OUTER_BOUND('',#2465,.T.);
#1688=FACE_OUTER_BOUND('',#2466,.T.);
#1689=FACE_OUTER_BOUND('',#2467,.T.);
#1690=FACE_OUTER_BOUND('',#2468,.T.);
#1691=FACE_OUTER_BOUND('',#2469,.T.);
#1692=FACE_OUTER_BOUND('',#2470,.T.);
#1693=FACE_OUTER_BOUND('',#2471,.T.);
#1694=FACE_OUTER_BOUND('',#2472,.T.);
#1695=FACE_OUTER_BOUND('',#2473,.T.);
#1696=FACE_OUTER_BOUND('',#2474,.T.);
#1697=FACE_OUTER_BOUND('',#2475,.T.);
#1698=FACE_OUTER_BOUND('',#2476,.T.);
#1699=FACE_OUTER_BOUND('',#2478,.T.);
#1700=FACE_OUTER_BOUND('',#2479,.T.);
#1701=FACE_OUTER_BOUND('',#2480,.T.);
#1702=FACE_OUTER_BOUND('',#2481,.T.);
#1703=FACE_OUTER_BOUND('',#2482,.T.);
#1704=FACE_OUTER_BOUND('',#2483,.T.);
#1705=FACE_OUTER_BOUND('',#2484,.T.);
#1706=FACE_OUTER_BOUND('',#2486,.T.);
#1707=FACE_OUTER_BOUND('',#2488,.T.);
#1708=FACE_OUTER_BOUND('',#2489,.T.);
#1709=FACE_OUTER_BOUND('',#2490,.T.);
#1710=FACE_OUTER_BOUND('',#2492,.T.);
#1711=FACE_OUTER_BOUND('',#2494,.T.);
#1712=FACE_OUTER_BOUND('',#2495,.T.);
#1713=FACE_OUTER_BOUND('',#2496,.T.);
#1714=FACE_OUTER_BOUND('',#2497,.T.);
#1715=FACE_OUTER_BOUND('',#2499,.T.);
#1716=FACE_OUTER_BOUND('',#2501,.T.);
#1717=FACE_OUTER_BOUND('',#2502,.T.);
#1718=FACE_OUTER_BOUND('',#2503,.T.);
#1719=FACE_OUTER_BOUND('',#2505,.T.);
#1720=FACE_OUTER_BOUND('',#2507,.T.);
#1721=FACE_OUTER_BOUND('',#2508,.T.);
#1722=FACE_OUTER_BOUND('',#2509,.T.);
#1723=FACE_OUTER_BOUND('',#2511,.T.);
#1724=FACE_OUTER_BOUND('',#2513,.T.);
#1725=FACE_OUTER_BOUND('',#2514,.T.);
#1726=FACE_OUTER_BOUND('',#2515,.T.);
#1727=FACE_OUTER_BOUND('',#2516,.T.);
#1728=FACE_OUTER_BOUND('',#2517,.T.);
#1729=FACE_OUTER_BOUND('',#2519,.T.);
#1730=FACE_OUTER_BOUND('',#2520,.T.);
#1731=FACE_OUTER_BOUND('',#2521,.T.);
#1732=FACE_OUTER_BOUND('',#2523,.T.);
#1733=FACE_OUTER_BOUND('',#2525,.T.);
#1734=FACE_OUTER_BOUND('',#2526,.T.);
#1735=FACE_OUTER_BOUND('',#2527,.T.);
#1736=FACE_OUTER_BOUND('',#2529,.T.);
#1737=FACE_OUTER_BOUND('',#2531,.T.);
#1738=FACE_OUTER_BOUND('',#2532,.T.);
#1739=FACE_OUTER_BOUND('',#2533,.T.);
#1740=FACE_OUTER_BOUND('',#2535,.T.);
#1741=FACE_OUTER_BOUND('',#2537,.T.);
#1742=FACE_OUTER_BOUND('',#2538,.T.);
#1743=FACE_OUTER_BOUND('',#2539,.T.);
#1744=FACE_OUTER_BOUND('',#2540,.T.);
#1745=FACE_OUTER_BOUND('',#2541,.T.);
#1746=FACE_OUTER_BOUND('',#2542,.T.);
#1747=FACE_OUTER_BOUND('',#2544,.T.);
#1748=FACE_OUTER_BOUND('',#2546,.T.);
#1749=FACE_OUTER_BOUND('',#2547,.T.);
#1750=FACE_OUTER_BOUND('',#2548,.T.);
#1751=FACE_OUTER_BOUND('',#2549,.T.);
#1752=FACE_OUTER_BOUND('',#2550,.T.);
#1753=FACE_OUTER_BOUND('',#2552,.T.);
#1754=FACE_OUTER_BOUND('',#2553,.T.);
#1755=FACE_OUTER_BOUND('',#2554,.T.);
#1756=FACE_OUTER_BOUND('',#2555,.T.);
#1757=FACE_OUTER_BOUND('',#2556,.T.);
#1758=FACE_OUTER_BOUND('',#2557,.T.);
#1759=FACE_OUTER_BOUND('',#2558,.T.);
#1760=FACE_OUTER_BOUND('',#2559,.T.);
#1761=FACE_OUTER_BOUND('',#2560,.T.);
#1762=FACE_OUTER_BOUND('',#2561,.T.);
#1763=FACE_OUTER_BOUND('',#2562,.T.);
#1764=FACE_OUTER_BOUND('',#2563,.T.);
#1765=FACE_OUTER_BOUND('',#2564,.T.);
#1766=FACE_OUTER_BOUND('',#2565,.T.);
#1767=FACE_OUTER_BOUND('',#2566,.T.);
#1768=FACE_OUTER_BOUND('',#2567,.T.);
#1769=FACE_OUTER_BOUND('',#2568,.T.);
#1770=FACE_OUTER_BOUND('',#2569,.T.);
#1771=FACE_OUTER_BOUND('',#2570,.T.);
#1772=FACE_OUTER_BOUND('',#2571,.T.);
#1773=FACE_OUTER_BOUND('',#2573,.T.);
#1774=FACE_OUTER_BOUND('',#2574,.T.);
#1775=FACE_OUTER_BOUND('',#2575,.T.);
#1776=FACE_OUTER_BOUND('',#2576,.T.);
#1777=EDGE_LOOP('',(#6103,#6104,#6105,#6106));
#1778=EDGE_LOOP('',(#6107,#6108,#6109,#6110));
#1779=EDGE_LOOP('',(#6111,#6112,#6113,#6114));
#1780=EDGE_LOOP('',(#6115,#6116,#6117,#6118));
#1781=EDGE_LOOP('',(#6119,#6120,#6121,#6122));
#1782=EDGE_LOOP('',(#6123,#6124,#6125,#6126));
#1783=EDGE_LOOP('',(#6127,#6128,#6129,#6130));
#1784=EDGE_LOOP('',(#6131,#6132,#6133,#6134));
#1785=EDGE_LOOP('',(#6135,#6136,#6137,#6138));
#1786=EDGE_LOOP('',(#6139,#6140,#6141,#6142));
#1787=EDGE_LOOP('',(#6143,#6144,#6145,#6146));
#1788=EDGE_LOOP('',(#6147,#6148,#6149,#6150));
#1789=EDGE_LOOP('',(#6151,#6152,#6153,#6154));
#1790=EDGE_LOOP('',(#6155,#6156,#6157,#6158));
#1791=EDGE_LOOP('',(#6159,#6160,#6161,#6162));
#1792=EDGE_LOOP('',(#6163,#6164,#6165,#6166));
#1793=EDGE_LOOP('',(#6167,#6168,#6169,#6170));
#1794=EDGE_LOOP('',(#6171));
#1795=EDGE_LOOP('',(#6172));
#1796=EDGE_LOOP('',(#6173));
#1797=EDGE_LOOP('',(#6174));
#1798=EDGE_LOOP('',(#6175));
#1799=EDGE_LOOP('',(#6176));
#1800=EDGE_LOOP('',(#6177));
#1801=EDGE_LOOP('',(#6178));
#1802=EDGE_LOOP('',(#6179));
#1803=EDGE_LOOP('',(#6180));
#1804=EDGE_LOOP('',(#6181));
#1805=EDGE_LOOP('',(#6182));
#1806=EDGE_LOOP('',(#6183,#6184,#6185,#6186));
#1807=EDGE_LOOP('',(#6187));
#1808=EDGE_LOOP('',(#6188));
#1809=EDGE_LOOP('',(#6189));
#1810=EDGE_LOOP('',(#6190));
#1811=EDGE_LOOP('',(#6191));
#1812=EDGE_LOOP('',(#6192));
#1813=EDGE_LOOP('',(#6193));
#1814=EDGE_LOOP('',(#6194));
#1815=EDGE_LOOP('',(#6195));
#1816=EDGE_LOOP('',(#6196));
#1817=EDGE_LOOP('',(#6197));
#1818=EDGE_LOOP('',(#6198));
#1819=EDGE_LOOP('',(#6199,#6200,#6201,#6202));
#1820=EDGE_LOOP('',(#6203,#6204,#6205,#6206));
#1821=EDGE_LOOP('',(#6207,#6208,#6209,#6210));
#1822=EDGE_LOOP('',(#6211,#6212,#6213,#6214));
#1823=EDGE_LOOP('',(#6215,#6216,#6217,#6218));
#1824=EDGE_LOOP('',(#6219,#6220,#6221,#6222));
#1825=EDGE_LOOP('',(#6223,#6224,#6225,#6226));
#1826=EDGE_LOOP('',(#6227,#6228,#6229,#6230));
#1827=EDGE_LOOP('',(#6231,#6232,#6233,#6234));
#1828=EDGE_LOOP('',(#6235,#6236,#6237,#6238));
#1829=EDGE_LOOP('',(#6239,#6240,#6241,#6242));
#1830=EDGE_LOOP('',(#6243,#6244,#6245,#6246));
#1831=EDGE_LOOP('',(#6247,#6248,#6249,#6250));
#1832=EDGE_LOOP('',(#6251,#6252,#6253,#6254));
#1833=EDGE_LOOP('',(#6255,#6256));
#1834=EDGE_LOOP('',(#6257,#6258,#6259,#6260,#6261,#6262,#6263,#6264,#6265));
#1835=EDGE_LOOP('',(#6266,#6267));
#1836=EDGE_LOOP('',(#6268,#6269,#6270,#6271));
#1837=EDGE_LOOP('',(#6272,#6273));
#1838=EDGE_LOOP('',(#6274));
#1839=EDGE_LOOP('',(#6275,#6276,#6277,#6278));
#1840=EDGE_LOOP('',(#6279,#6280));
#1841=EDGE_LOOP('',(#6281));
#1842=EDGE_LOOP('',(#6282,#6283,#6284,#6285,#6286,#6287,#6288,#6289,#6290,
#6291));
#1843=EDGE_LOOP('',(#6292));
#1844=EDGE_LOOP('',(#6293,#6294,#6295,#6296));
#1845=EDGE_LOOP('',(#6297,#6298,#6299,#6300));
#1846=EDGE_LOOP('',(#6301,#6302,#6303,#6304,#6305,#6306,#6307,#6308,#6309,
#6310,#6311,#6312));
#1847=EDGE_LOOP('',(#6313,#6314,#6315,#6316,#6317,#6318,#6319));
#1848=EDGE_LOOP('',(#6320,#6321,#6322,#6323));
#1849=EDGE_LOOP('',(#6324));
#1850=EDGE_LOOP('',(#6325,#6326,#6327,#6328,#6329,#6330,#6331));
#1851=EDGE_LOOP('',(#6332,#6333,#6334,#6335));
#1852=EDGE_LOOP('',(#6336));
#1853=EDGE_LOOP('',(#6337,#6338,#6339,#6340));
#1854=EDGE_LOOP('',(#6341));
#1855=EDGE_LOOP('',(#6342));
#1856=EDGE_LOOP('',(#6343,#6344,#6345,#6346));
#1857=EDGE_LOOP('',(#6347,#6348,#6349,#6350));
#1858=EDGE_LOOP('',(#6351,#6352));
#1859=EDGE_LOOP('',(#6353,#6354,#6355,#6356,#6357,#6358,#6359,#6360,#6361));
#1860=EDGE_LOOP('',(#6362,#6363));
#1861=EDGE_LOOP('',(#6364,#6365,#6366,#6367));
#1862=EDGE_LOOP('',(#6368,#6369));
#1863=EDGE_LOOP('',(#6370));
#1864=EDGE_LOOP('',(#6371,#6372,#6373,#6374));
#1865=EDGE_LOOP('',(#6375,#6376));
#1866=EDGE_LOOP('',(#6377));
#1867=EDGE_LOOP('',(#6378,#6379,#6380,#6381,#6382,#6383,#6384,#6385,#6386,
#6387));
#1868=EDGE_LOOP('',(#6388));
#1869=EDGE_LOOP('',(#6389,#6390,#6391,#6392));
#1870=EDGE_LOOP('',(#6393,#6394,#6395,#6396));
#1871=EDGE_LOOP('',(#6397,#6398,#6399,#6400,#6401,#6402,#6403,#6404,#6405,
#6406,#6407,#6408));
#1872=EDGE_LOOP('',(#6409,#6410,#6411,#6412,#6413,#6414,#6415));
#1873=EDGE_LOOP('',(#6416,#6417,#6418,#6419));
#1874=EDGE_LOOP('',(#6420));
#1875=EDGE_LOOP('',(#6421,#6422,#6423,#6424,#6425,#6426,#6427));
#1876=EDGE_LOOP('',(#6428,#6429,#6430,#6431));
#1877=EDGE_LOOP('',(#6432));
#1878=EDGE_LOOP('',(#6433,#6434,#6435,#6436));
#1879=EDGE_LOOP('',(#6437));
#1880=EDGE_LOOP('',(#6438));
#1881=EDGE_LOOP('',(#6439,#6440,#6441,#6442));
#1882=EDGE_LOOP('',(#6443,#6444,#6445,#6446));
#1883=EDGE_LOOP('',(#6447,#6448));
#1884=EDGE_LOOP('',(#6449,#6450,#6451,#6452,#6453,#6454,#6455,#6456,#6457));
#1885=EDGE_LOOP('',(#6458,#6459));
#1886=EDGE_LOOP('',(#6460,#6461,#6462,#6463));
#1887=EDGE_LOOP('',(#6464,#6465));
#1888=EDGE_LOOP('',(#6466));
#1889=EDGE_LOOP('',(#6467,#6468,#6469,#6470));
#1890=EDGE_LOOP('',(#6471,#6472));
#1891=EDGE_LOOP('',(#6473));
#1892=EDGE_LOOP('',(#6474,#6475,#6476,#6477,#6478,#6479,#6480,#6481,#6482,
#6483));
#1893=EDGE_LOOP('',(#6484));
#1894=EDGE_LOOP('',(#6485,#6486,#6487,#6488));
#1895=EDGE_LOOP('',(#6489,#6490,#6491,#6492));
#1896=EDGE_LOOP('',(#6493,#6494,#6495,#6496,#6497,#6498,#6499,#6500,#6501,
#6502,#6503,#6504));
#1897=EDGE_LOOP('',(#6505,#6506,#6507,#6508,#6509,#6510,#6511));
#1898=EDGE_LOOP('',(#6512,#6513,#6514,#6515));
#1899=EDGE_LOOP('',(#6516));
#1900=EDGE_LOOP('',(#6517,#6518,#6519,#6520,#6521,#6522,#6523));
#1901=EDGE_LOOP('',(#6524,#6525,#6526,#6527));
#1902=EDGE_LOOP('',(#6528));
#1903=EDGE_LOOP('',(#6529,#6530,#6531,#6532));
#1904=EDGE_LOOP('',(#6533));
#1905=EDGE_LOOP('',(#6534));
#1906=EDGE_LOOP('',(#6535,#6536,#6537,#6538));
#1907=EDGE_LOOP('',(#6539,#6540,#6541,#6542));
#1908=EDGE_LOOP('',(#6543,#6544));
#1909=EDGE_LOOP('',(#6545,#6546,#6547,#6548,#6549,#6550,#6551,#6552,#6553));
#1910=EDGE_LOOP('',(#6554,#6555));
#1911=EDGE_LOOP('',(#6556,#6557,#6558,#6559));
#1912=EDGE_LOOP('',(#6560,#6561));
#1913=EDGE_LOOP('',(#6562));
#1914=EDGE_LOOP('',(#6563,#6564,#6565,#6566));
#1915=EDGE_LOOP('',(#6567,#6568));
#1916=EDGE_LOOP('',(#6569));
#1917=EDGE_LOOP('',(#6570,#6571,#6572,#6573,#6574,#6575,#6576,#6577,#6578,
#6579));
#1918=EDGE_LOOP('',(#6580));
#1919=EDGE_LOOP('',(#6581,#6582,#6583,#6584));
#1920=EDGE_LOOP('',(#6585,#6586,#6587,#6588));
#1921=EDGE_LOOP('',(#6589,#6590,#6591,#6592,#6593,#6594,#6595,#6596,#6597,
#6598,#6599,#6600));
#1922=EDGE_LOOP('',(#6601,#6602,#6603,#6604,#6605,#6606,#6607));
#1923=EDGE_LOOP('',(#6608,#6609,#6610,#6611));
#1924=EDGE_LOOP('',(#6612));
#1925=EDGE_LOOP('',(#6613,#6614,#6615,#6616,#6617,#6618,#6619));
#1926=EDGE_LOOP('',(#6620,#6621,#6622,#6623));
#1927=EDGE_LOOP('',(#6624));
#1928=EDGE_LOOP('',(#6625,#6626,#6627,#6628));
#1929=EDGE_LOOP('',(#6629));
#1930=EDGE_LOOP('',(#6630));
#1931=EDGE_LOOP('',(#6631,#6632,#6633,#6634));
#1932=EDGE_LOOP('',(#6635,#6636,#6637,#6638));
#1933=EDGE_LOOP('',(#6639,#6640,#6641,#6642));
#1934=EDGE_LOOP('',(#6643,#6644,#6645,#6646));
#1935=EDGE_LOOP('',(#6647,#6648,#6649,#6650));
#1936=EDGE_LOOP('',(#6651,#6652,#6653,#6654));
#1937=EDGE_LOOP('',(#6655,#6656,#6657,#6658));
#1938=EDGE_LOOP('',(#6659,#6660,#6661,#6662));
#1939=EDGE_LOOP('',(#6663));
#1940=EDGE_LOOP('',(#6664,#6665,#6666,#6667));
#1941=EDGE_LOOP('',(#6668));
#1942=EDGE_LOOP('',(#6669,#6670,#6671,#6672));
#1943=EDGE_LOOP('',(#6673,#6674,#6675,#6676));
#1944=EDGE_LOOP('',(#6677,#6678,#6679,#6680));
#1945=EDGE_LOOP('',(#6681,#6682,#6683,#6684,#6685,#6686,#6687,#6688));
#1946=EDGE_LOOP('',(#6689));
#1947=EDGE_LOOP('',(#6690));
#1948=EDGE_LOOP('',(#6691));
#1949=EDGE_LOOP('',(#6692));
#1950=EDGE_LOOP('',(#6693));
#1951=EDGE_LOOP('',(#6694,#6695,#6696,#6697));
#1952=EDGE_LOOP('',(#6698,#6699,#6700,#6701,#6702,#6703,#6704,#6705));
#1953=EDGE_LOOP('',(#6706));
#1954=EDGE_LOOP('',(#6707));
#1955=EDGE_LOOP('',(#6708));
#1956=EDGE_LOOP('',(#6709));
#1957=EDGE_LOOP('',(#6710));
#1958=EDGE_LOOP('',(#6711,#6712,#6713,#6714));
#1959=EDGE_LOOP('',(#6715,#6716,#6717,#6718));
#1960=EDGE_LOOP('',(#6719));
#1961=EDGE_LOOP('',(#6720));
#1962=EDGE_LOOP('',(#6721,#6722,#6723,#6724));
#1963=EDGE_LOOP('',(#6725,#6726,#6727,#6728));
#1964=EDGE_LOOP('',(#6729,#6730,#6731,#6732));
#1965=EDGE_LOOP('',(#6733,#6734,#6735,#6736));
#1966=EDGE_LOOP('',(#6737,#6738,#6739,#6740));
#1967=EDGE_LOOP('',(#6741));
#1968=EDGE_LOOP('',(#6742));
#1969=EDGE_LOOP('',(#6743,#6744,#6745,#6746));
#1970=EDGE_LOOP('',(#6747,#6748,#6749,#6750));
#1971=EDGE_LOOP('',(#6751));
#1972=EDGE_LOOP('',(#6752));
#1973=EDGE_LOOP('',(#6753));
#1974=EDGE_LOOP('',(#6754));
#1975=EDGE_LOOP('',(#6755));
#1976=EDGE_LOOP('',(#6756));
#1977=EDGE_LOOP('',(#6757));
#1978=EDGE_LOOP('',(#6758));
#1979=EDGE_LOOP('',(#6759));
#1980=EDGE_LOOP('',(#6760));
#1981=EDGE_LOOP('',(#6761));
#1982=EDGE_LOOP('',(#6762));
#1983=EDGE_LOOP('',(#6763,#6764,#6765,#6766));
#1984=EDGE_LOOP('',(#6767,#6768,#6769,#6770));
#1985=EDGE_LOOP('',(#6771,#6772,#6773,#6774));
#1986=EDGE_LOOP('',(#6775,#6776,#6777,#6778));
#1987=EDGE_LOOP('',(#6779,#6780,#6781,#6782));
#1988=EDGE_LOOP('',(#6783));
#1989=EDGE_LOOP('',(#6784));
#1990=EDGE_LOOP('',(#6785,#6786,#6787,#6788));
#1991=EDGE_LOOP('',(#6789,#6790,#6791,#6792));
#1992=EDGE_LOOP('',(#6793));
#1993=EDGE_LOOP('',(#6794));
#1994=EDGE_LOOP('',(#6795));
#1995=EDGE_LOOP('',(#6796));
#1996=EDGE_LOOP('',(#6797));
#1997=EDGE_LOOP('',(#6798));
#1998=EDGE_LOOP('',(#6799));
#1999=EDGE_LOOP('',(#6800));
#2000=EDGE_LOOP('',(#6801));
#2001=EDGE_LOOP('',(#6802));
#2002=EDGE_LOOP('',(#6803));
#2003=EDGE_LOOP('',(#6804));
#2004=EDGE_LOOP('',(#6805,#6806,#6807,#6808));
#2005=EDGE_LOOP('',(#6809,#6810,#6811,#6812));
#2006=EDGE_LOOP('',(#6813,#6814,#6815,#6816));
#2007=EDGE_LOOP('',(#6817,#6818,#6819,#6820));
#2008=EDGE_LOOP('',(#6821,#6822,#6823,#6824));
#2009=EDGE_LOOP('',(#6825,#6826,#6827,#6828));
#2010=EDGE_LOOP('',(#6829,#6830,#6831,#6832));
#2011=EDGE_LOOP('',(#6833,#6834,#6835,#6836));
#2012=EDGE_LOOP('',(#6837));
#2013=EDGE_LOOP('',(#6838,#6839,#6840,#6841));
#2014=EDGE_LOOP('',(#6842));
#2015=EDGE_LOOP('',(#6843,#6844,#6845,#6846));
#2016=EDGE_LOOP('',(#6847,#6848,#6849,#6850));
#2017=EDGE_LOOP('',(#6851,#6852,#6853,#6854));
#2018=EDGE_LOOP('',(#6855,#6856,#6857,#6858,#6859,#6860,#6861,#6862));
#2019=EDGE_LOOP('',(#6863));
#2020=EDGE_LOOP('',(#6864));
#2021=EDGE_LOOP('',(#6865));
#2022=EDGE_LOOP('',(#6866));
#2023=EDGE_LOOP('',(#6867));
#2024=EDGE_LOOP('',(#6868,#6869,#6870,#6871));
#2025=EDGE_LOOP('',(#6872,#6873,#6874,#6875,#6876,#6877,#6878,#6879));
#2026=EDGE_LOOP('',(#6880));
#2027=EDGE_LOOP('',(#6881));
#2028=EDGE_LOOP('',(#6882));
#2029=EDGE_LOOP('',(#6883));
#2030=EDGE_LOOP('',(#6884));
#2031=EDGE_LOOP('',(#6885,#6886,#6887,#6888));
#2032=EDGE_LOOP('',(#6889,#6890,#6891,#6892));
#2033=EDGE_LOOP('',(#6893));
#2034=EDGE_LOOP('',(#6894));
#2035=EDGE_LOOP('',(#6895,#6896,#6897,#6898));
#2036=EDGE_LOOP('',(#6899,#6900,#6901,#6902));
#2037=EDGE_LOOP('',(#6903,#6904,#6905,#6906));
#2038=EDGE_LOOP('',(#6907,#6908,#6909,#6910));
#2039=EDGE_LOOP('',(#6911,#6912,#6913,#6914));
#2040=EDGE_LOOP('',(#6915));
#2041=EDGE_LOOP('',(#6916));
#2042=EDGE_LOOP('',(#6917,#6918,#6919,#6920));
#2043=EDGE_LOOP('',(#6921,#6922,#6923,#6924));
#2044=EDGE_LOOP('',(#6925));
#2045=EDGE_LOOP('',(#6926));
#2046=EDGE_LOOP('',(#6927));
#2047=EDGE_LOOP('',(#6928));
#2048=EDGE_LOOP('',(#6929));
#2049=EDGE_LOOP('',(#6930));
#2050=EDGE_LOOP('',(#6931));
#2051=EDGE_LOOP('',(#6932));
#2052=EDGE_LOOP('',(#6933));
#2053=EDGE_LOOP('',(#6934));
#2054=EDGE_LOOP('',(#6935));
#2055=EDGE_LOOP('',(#6936));
#2056=EDGE_LOOP('',(#6937,#6938,#6939,#6940));
#2057=EDGE_LOOP('',(#6941,#6942,#6943,#6944));
#2058=EDGE_LOOP('',(#6945,#6946,#6947,#6948));
#2059=EDGE_LOOP('',(#6949,#6950,#6951,#6952));
#2060=EDGE_LOOP('',(#6953,#6954,#6955,#6956));
#2061=EDGE_LOOP('',(#6957));
#2062=EDGE_LOOP('',(#6958));
#2063=EDGE_LOOP('',(#6959,#6960,#6961,#6962));
#2064=EDGE_LOOP('',(#6963,#6964,#6965,#6966));
#2065=EDGE_LOOP('',(#6967));
#2066=EDGE_LOOP('',(#6968));
#2067=EDGE_LOOP('',(#6969));
#2068=EDGE_LOOP('',(#6970));
#2069=EDGE_LOOP('',(#6971));
#2070=EDGE_LOOP('',(#6972));
#2071=EDGE_LOOP('',(#6973));
#2072=EDGE_LOOP('',(#6974));
#2073=EDGE_LOOP('',(#6975));
#2074=EDGE_LOOP('',(#6976));
#2075=EDGE_LOOP('',(#6977));
#2076=EDGE_LOOP('',(#6978));
#2077=EDGE_LOOP('',(#6979,#6980,#6981,#6982));
#2078=EDGE_LOOP('',(#6983,#6984,#6985,#6986));
#2079=EDGE_LOOP('',(#6987));
#2080=EDGE_LOOP('',(#6988,#6989,#6990,#6991));
#2081=EDGE_LOOP('',(#6992));
#2082=EDGE_LOOP('',(#6993,#6994,#6995,#6996,#6997,#6998));
#2083=EDGE_LOOP('',(#6999,#7000,#7001,#7002,#7003));
#2084=EDGE_LOOP('',(#7004,#7005,#7006,#7007));
#2085=EDGE_LOOP('',(#7008,#7009,#7010,#7011));
#2086=EDGE_LOOP('',(#7012));
#2087=EDGE_LOOP('',(#7013));
#2088=EDGE_LOOP('',(#7014,#7015,#7016,#7017,#7018));
#2089=EDGE_LOOP('',(#7019));
#2090=EDGE_LOOP('',(#7020));
#2091=EDGE_LOOP('',(#7021,#7022,#7023,#7024));
#2092=EDGE_LOOP('',(#7025,#7026,#7027,#7028,#7029,#7030));
#2093=EDGE_LOOP('',(#7031,#7032,#7033,#7034,#7035));
#2094=EDGE_LOOP('',(#7036));
#2095=EDGE_LOOP('',(#7037));
#2096=EDGE_LOOP('',(#7038,#7039,#7040,#7041));
#2097=EDGE_LOOP('',(#7042,#7043,#7044,#7045));
#2098=EDGE_LOOP('',(#7046,#7047,#7048,#7049));
#2099=EDGE_LOOP('',(#7050));
#2100=EDGE_LOOP('',(#7051));
#2101=EDGE_LOOP('',(#7052,#7053,#7054,#7055,#7056));
#2102=EDGE_LOOP('',(#7057,#7058));
#2103=EDGE_LOOP('',(#7059,#7060));
#2104=EDGE_LOOP('',(#7061,#7062));
#2105=EDGE_LOOP('',(#7063,#7064));
#2106=EDGE_LOOP('',(#7065,#7066));
#2107=EDGE_LOOP('',(#7067,#7068));
#2108=EDGE_LOOP('',(#7069,#7070));
#2109=EDGE_LOOP('',(#7071,#7072,#7073,#7074));
#2110=EDGE_LOOP('',(#7075,#7076,#7077,#7078,#7079,#7080,#7081,#7082,#7083,
#7084,#7085,#7086,#7087,#7088,#7089,#7090,#7091,#7092));
#2111=EDGE_LOOP('',(#7093,#7094,#7095,#7096));
#2112=EDGE_LOOP('',(#7097,#7098,#7099,#7100));
#2113=EDGE_LOOP('',(#7101,#7102,#7103,#7104));
#2114=EDGE_LOOP('',(#7105,#7106,#7107,#7108));
#2115=EDGE_LOOP('',(#7109,#7110,#7111,#7112,#7113,#7114));
#2116=EDGE_LOOP('',(#7115,#7116,#7117,#7118));
#2117=EDGE_LOOP('',(#7119,#7120,#7121,#7122));
#2118=EDGE_LOOP('',(#7123,#7124,#7125,#7126));
#2119=EDGE_LOOP('',(#7127,#7128,#7129,#7130));
#2120=EDGE_LOOP('',(#7131,#7132,#7133,#7134));
#2121=EDGE_LOOP('',(#7135,#7136,#7137,#7138,#7139,#7140,#7141,#7142,#7143,
#7144,#7145,#7146,#7147,#7148,#7149,#7150,#7151,#7152));
#2122=EDGE_LOOP('',(#7153,#7154,#7155,#7156));
#2123=EDGE_LOOP('',(#7157,#7158,#7159,#7160));
#2124=EDGE_LOOP('',(#7161));
#2125=EDGE_LOOP('',(#7162));
#2126=EDGE_LOOP('',(#7163,#7164,#7165,#7166));
#2127=EDGE_LOOP('',(#7167));
#2128=EDGE_LOOP('',(#7168));
#2129=EDGE_LOOP('',(#7169,#7170,#7171,#7172));
#2130=EDGE_LOOP('',(#7173));
#2131=EDGE_LOOP('',(#7174));
#2132=EDGE_LOOP('',(#7175,#7176,#7177,#7178));
#2133=EDGE_LOOP('',(#7179));
#2134=EDGE_LOOP('',(#7180));
#2135=EDGE_LOOP('',(#7181,#7182,#7183,#7184));
#2136=EDGE_LOOP('',(#7185));
#2137=EDGE_LOOP('',(#7186));
#2138=EDGE_LOOP('',(#7187,#7188,#7189,#7190));
#2139=EDGE_LOOP('',(#7191,#7192,#7193,#7194));
#2140=EDGE_LOOP('',(#7195));
#2141=EDGE_LOOP('',(#7196,#7197,#7198,#7199));
#2142=EDGE_LOOP('',(#7200));
#2143=EDGE_LOOP('',(#7201,#7202,#7203,#7204));
#2144=EDGE_LOOP('',(#7205));
#2145=EDGE_LOOP('',(#7206,#7207,#7208,#7209));
#2146=EDGE_LOOP('',(#7210));
#2147=EDGE_LOOP('',(#7211,#7212,#7213,#7214));
#2148=EDGE_LOOP('',(#7215));
#2149=EDGE_LOOP('',(#7216,#7217,#7218,#7219));
#2150=EDGE_LOOP('',(#7220));
#2151=EDGE_LOOP('',(#7221,#7222,#7223,#7224));
#2152=EDGE_LOOP('',(#7225,#7226,#7227,#7228));
#2153=EDGE_LOOP('',(#7229,#7230,#7231,#7232));
#2154=EDGE_LOOP('',(#7233,#7234,#7235,#7236));
#2155=EDGE_LOOP('',(#7237,#7238,#7239,#7240));
#2156=EDGE_LOOP('',(#7241,#7242,#7243,#7244));
#2157=EDGE_LOOP('',(#7245,#7246,#7247,#7248));
#2158=EDGE_LOOP('',(#7249,#7250,#7251,#7252));
#2159=EDGE_LOOP('',(#7253,#7254,#7255,#7256));
#2160=EDGE_LOOP('',(#7257));
#2161=EDGE_LOOP('',(#7258));
#2162=EDGE_LOOP('',(#7259));
#2163=EDGE_LOOP('',(#7260));
#2164=EDGE_LOOP('',(#7261));
#2165=EDGE_LOOP('',(#7262));
#2166=EDGE_LOOP('',(#7263));
#2167=EDGE_LOOP('',(#7264));
#2168=EDGE_LOOP('',(#7265));
#2169=EDGE_LOOP('',(#7266));
#2170=EDGE_LOOP('',(#7267));
#2171=EDGE_LOOP('',(#7268));
#2172=EDGE_LOOP('',(#7269));
#2173=EDGE_LOOP('',(#7270,#7271,#7272,#7273));
#2174=EDGE_LOOP('',(#7274,#7275,#7276,#7277));
#2175=EDGE_LOOP('',(#7278));
#2176=EDGE_LOOP('',(#7279));
#2177=EDGE_LOOP('',(#7280));
#2178=EDGE_LOOP('',(#7281));
#2179=EDGE_LOOP('',(#7282));
#2180=EDGE_LOOP('',(#7283));
#2181=EDGE_LOOP('',(#7284));
#2182=EDGE_LOOP('',(#7285,#7286,#7287,#7288));
#2183=EDGE_LOOP('',(#7289,#7290,#7291,#7292));
#2184=EDGE_LOOP('',(#7293,#7294,#7295,#7296));
#2185=EDGE_LOOP('',(#7297,#7298,#7299,#7300));
#2186=EDGE_LOOP('',(#7301,#7302,#7303,#7304));
#2187=EDGE_LOOP('',(#7305,#7306,#7307,#7308));
#2188=EDGE_LOOP('',(#7309,#7310,#7311,#7312));
#2189=EDGE_LOOP('',(#7313,#7314,#7315,#7316));
#2190=EDGE_LOOP('',(#7317,#7318,#7319,#7320));
#2191=EDGE_LOOP('',(#7321,#7322,#7323,#7324));
#2192=EDGE_LOOP('',(#7325,#7326,#7327,#7328));
#2193=EDGE_LOOP('',(#7329));
#2194=EDGE_LOOP('',(#7330));
#2195=EDGE_LOOP('',(#7331));
#2196=EDGE_LOOP('',(#7332));
#2197=EDGE_LOOP('',(#7333));
#2198=EDGE_LOOP('',(#7334));
#2199=EDGE_LOOP('',(#7335));
#2200=EDGE_LOOP('',(#7336,#7337,#7338,#7339));
#2201=EDGE_LOOP('',(#7340,#7341,#7342,#7343));
#2202=EDGE_LOOP('',(#7344));
#2203=EDGE_LOOP('',(#7345));
#2204=EDGE_LOOP('',(#7346));
#2205=EDGE_LOOP('',(#7347));
#2206=EDGE_LOOP('',(#7348));
#2207=EDGE_LOOP('',(#7349));
#2208=EDGE_LOOP('',(#7350));
#2209=EDGE_LOOP('',(#7351,#7352,#7353,#7354));
#2210=EDGE_LOOP('',(#7355,#7356,#7357,#7358));
#2211=EDGE_LOOP('',(#7359,#7360,#7361,#7362));
#2212=EDGE_LOOP('',(#7363,#7364,#7365,#7366));
#2213=EDGE_LOOP('',(#7367,#7368,#7369,#7370));
#2214=EDGE_LOOP('',(#7371,#7372,#7373,#7374));
#2215=EDGE_LOOP('',(#7375,#7376,#7377,#7378));
#2216=EDGE_LOOP('',(#7379,#7380,#7381,#7382));
#2217=EDGE_LOOP('',(#7383,#7384,#7385,#7386));
#2218=EDGE_LOOP('',(#7387,#7388,#7389,#7390));
#2219=EDGE_LOOP('',(#7391,#7392,#7393,#7394));
#2220=EDGE_LOOP('',(#7395));
#2221=EDGE_LOOP('',(#7396));
#2222=EDGE_LOOP('',(#7397));
#2223=EDGE_LOOP('',(#7398));
#2224=EDGE_LOOP('',(#7399));
#2225=EDGE_LOOP('',(#7400));
#2226=EDGE_LOOP('',(#7401));
#2227=EDGE_LOOP('',(#7402,#7403,#7404,#7405));
#2228=EDGE_LOOP('',(#7406,#7407,#7408,#7409));
#2229=EDGE_LOOP('',(#7410));
#2230=EDGE_LOOP('',(#7411));
#2231=EDGE_LOOP('',(#7412));
#2232=EDGE_LOOP('',(#7413));
#2233=EDGE_LOOP('',(#7414));
#2234=EDGE_LOOP('',(#7415));
#2235=EDGE_LOOP('',(#7416));
#2236=EDGE_LOOP('',(#7417,#7418,#7419,#7420));
#2237=EDGE_LOOP('',(#7421,#7422,#7423,#7424));
#2238=EDGE_LOOP('',(#7425,#7426,#7427));
#2239=EDGE_LOOP('',(#7428,#7429,#7430,#7431,#7432,#7433,#7434,#7435));
#2240=EDGE_LOOP('',(#7436,#7437,#7438));
#2241=EDGE_LOOP('',(#7439,#7440,#7441,#7442,#7443,#7444,#7445,#7446));
#2242=EDGE_LOOP('',(#7447,#7448,#7449,#7450,#7451,#7452,#7453,#7454,#7455,
#7456,#7457,#7458));
#2243=EDGE_LOOP('',(#7459));
#2244=EDGE_LOOP('',(#7460,#7461,#7462,#7463,#7464));
#2245=EDGE_LOOP('',(#7465,#7466,#7467,#7468));
#2246=EDGE_LOOP('',(#7469));
#2247=EDGE_LOOP('',(#7470));
#2248=EDGE_LOOP('',(#7471));
#2249=EDGE_LOOP('',(#7472));
#2250=EDGE_LOOP('',(#7473,#7474,#7475,#7476));
#2251=EDGE_LOOP('',(#7477));
#2252=EDGE_LOOP('',(#7478));
#2253=EDGE_LOOP('',(#7479,#7480,#7481,#7482));
#2254=EDGE_LOOP('',(#7483));
#2255=EDGE_LOOP('',(#7484));
#2256=EDGE_LOOP('',(#7485,#7486,#7487,#7488));
#2257=EDGE_LOOP('',(#7489));
#2258=EDGE_LOOP('',(#7490));
#2259=EDGE_LOOP('',(#7491,#7492,#7493,#7494));
#2260=EDGE_LOOP('',(#7495));
#2261=EDGE_LOOP('',(#7496));
#2262=EDGE_LOOP('',(#7497,#7498,#7499,#7500));
#2263=EDGE_LOOP('',(#7501));
#2264=EDGE_LOOP('',(#7502));
#2265=EDGE_LOOP('',(#7503,#7504,#7505,#7506));
#2266=EDGE_LOOP('',(#7507,#7508,#7509,#7510));
#2267=EDGE_LOOP('',(#7511,#7512,#7513,#7514));
#2268=EDGE_LOOP('',(#7515,#7516,#7517,#7518));
#2269=EDGE_LOOP('',(#7519,#7520,#7521,#7522));
#2270=EDGE_LOOP('',(#7523,#7524,#7525,#7526));
#2271=EDGE_LOOP('',(#7527));
#2272=EDGE_LOOP('',(#7528));
#2273=EDGE_LOOP('',(#7529));
#2274=EDGE_LOOP('',(#7530));
#2275=EDGE_LOOP('',(#7531,#7532,#7533,#7534));
#2276=EDGE_LOOP('',(#7535,#7536,#7537,#7538));
#2277=EDGE_LOOP('',(#7539));
#2278=EDGE_LOOP('',(#7540));
#2279=EDGE_LOOP('',(#7541));
#2280=EDGE_LOOP('',(#7542));
#2281=EDGE_LOOP('',(#7543,#7544,#7545,#7546));
#2282=EDGE_LOOP('',(#7547,#7548,#7549,#7550));
#2283=EDGE_LOOP('',(#7551,#7552,#7553,#7554));
#2284=EDGE_LOOP('',(#7555));
#2285=EDGE_LOOP('',(#7556,#7557,#7558,#7559));
#2286=EDGE_LOOP('',(#7560));
#2287=EDGE_LOOP('',(#7561,#7562,#7563,#7564));
#2288=EDGE_LOOP('',(#7565));
#2289=EDGE_LOOP('',(#7566,#7567,#7568,#7569));
#2290=EDGE_LOOP('',(#7570));
#2291=EDGE_LOOP('',(#7571,#7572,#7573,#7574));
#2292=EDGE_LOOP('',(#7575));
#2293=EDGE_LOOP('',(#7576,#7577,#7578,#7579));
#2294=EDGE_LOOP('',(#7580));
#2295=EDGE_LOOP('',(#7581,#7582,#7583,#7584));
#2296=EDGE_LOOP('',(#7585,#7586,#7587,#7588));
#2297=EDGE_LOOP('',(#7589,#7590,#7591,#7592));
#2298=EDGE_LOOP('',(#7593,#7594,#7595,#7596));
#2299=EDGE_LOOP('',(#7597,#7598,#7599,#7600));
#2300=EDGE_LOOP('',(#7601,#7602,#7603,#7604));
#2301=EDGE_LOOP('',(#7605,#7606,#7607,#7608));
#2302=EDGE_LOOP('',(#7609,#7610,#7611,#7612));
#2303=EDGE_LOOP('',(#7613,#7614,#7615,#7616));
#2304=EDGE_LOOP('',(#7617));
#2305=EDGE_LOOP('',(#7618));
#2306=EDGE_LOOP('',(#7619));
#2307=EDGE_LOOP('',(#7620));
#2308=EDGE_LOOP('',(#7621));
#2309=EDGE_LOOP('',(#7622));
#2310=EDGE_LOOP('',(#7623));
#2311=EDGE_LOOP('',(#7624,#7625,#7626,#7627));
#2312=EDGE_LOOP('',(#7628,#7629,#7630,#7631));
#2313=EDGE_LOOP('',(#7632));
#2314=EDGE_LOOP('',(#7633));
#2315=EDGE_LOOP('',(#7634));
#2316=EDGE_LOOP('',(#7635));
#2317=EDGE_LOOP('',(#7636));
#2318=EDGE_LOOP('',(#7637));
#2319=EDGE_LOOP('',(#7638));
#2320=EDGE_LOOP('',(#7639));
#2321=EDGE_LOOP('',(#7640));
#2322=EDGE_LOOP('',(#7641));
#2323=EDGE_LOOP('',(#7642));
#2324=EDGE_LOOP('',(#7643));
#2325=EDGE_LOOP('',(#7644));
#2326=EDGE_LOOP('',(#7645,#7646,#7647,#7648));
#2327=EDGE_LOOP('',(#7649,#7650,#7651,#7652));
#2328=EDGE_LOOP('',(#7653,#7654,#7655,#7656));
#2329=EDGE_LOOP('',(#7657,#7658,#7659,#7660));
#2330=EDGE_LOOP('',(#7661,#7662,#7663,#7664));
#2331=EDGE_LOOP('',(#7665,#7666,#7667,#7668));
#2332=EDGE_LOOP('',(#7669,#7670,#7671,#7672));
#2333=EDGE_LOOP('',(#7673,#7674,#7675,#7676));
#2334=EDGE_LOOP('',(#7677,#7678,#7679,#7680));
#2335=EDGE_LOOP('',(#7681,#7682,#7683,#7684));
#2336=EDGE_LOOP('',(#7685,#7686,#7687,#7688));
#2337=EDGE_LOOP('',(#7689));
#2338=EDGE_LOOP('',(#7690));
#2339=EDGE_LOOP('',(#7691));
#2340=EDGE_LOOP('',(#7692));
#2341=EDGE_LOOP('',(#7693));
#2342=EDGE_LOOP('',(#7694));
#2343=EDGE_LOOP('',(#7695));
#2344=EDGE_LOOP('',(#7696,#7697,#7698,#7699));
#2345=EDGE_LOOP('',(#7700,#7701,#7702,#7703));
#2346=EDGE_LOOP('',(#7704));
#2347=EDGE_LOOP('',(#7705));
#2348=EDGE_LOOP('',(#7706));
#2349=EDGE_LOOP('',(#7707));
#2350=EDGE_LOOP('',(#7708));
#2351=EDGE_LOOP('',(#7709));
#2352=EDGE_LOOP('',(#7710));
#2353=EDGE_LOOP('',(#7711,#7712,#7713,#7714));
#2354=EDGE_LOOP('',(#7715,#7716,#7717,#7718));
#2355=EDGE_LOOP('',(#7719,#7720,#7721,#7722));
#2356=EDGE_LOOP('',(#7723,#7724,#7725,#7726));
#2357=EDGE_LOOP('',(#7727,#7728,#7729,#7730));
#2358=EDGE_LOOP('',(#7731,#7732,#7733,#7734));
#2359=EDGE_LOOP('',(#7735,#7736,#7737,#7738));
#2360=EDGE_LOOP('',(#7739,#7740,#7741,#7742));
#2361=EDGE_LOOP('',(#7743,#7744,#7745,#7746));
#2362=EDGE_LOOP('',(#7747,#7748,#7749,#7750));
#2363=EDGE_LOOP('',(#7751,#7752,#7753,#7754));
#2364=EDGE_LOOP('',(#7755));
#2365=EDGE_LOOP('',(#7756));
#2366=EDGE_LOOP('',(#7757));
#2367=EDGE_LOOP('',(#7758));
#2368=EDGE_LOOP('',(#7759));
#2369=EDGE_LOOP('',(#7760));
#2370=EDGE_LOOP('',(#7761));
#2371=EDGE_LOOP('',(#7762,#7763,#7764,#7765));
#2372=EDGE_LOOP('',(#7766,#7767,#7768,#7769));
#2373=EDGE_LOOP('',(#7770));
#2374=EDGE_LOOP('',(#7771));
#2375=EDGE_LOOP('',(#7772));
#2376=EDGE_LOOP('',(#7773));
#2377=EDGE_LOOP('',(#7774));
#2378=EDGE_LOOP('',(#7775));
#2379=EDGE_LOOP('',(#7776));
#2380=EDGE_LOOP('',(#7777,#7778,#7779,#7780));
#2381=EDGE_LOOP('',(#7781,#7782,#7783,#7784));
#2382=EDGE_LOOP('',(#7785,#7786,#7787));
#2383=EDGE_LOOP('',(#7788,#7789,#7790,#7791,#7792,#7793,#7794,#7795));
#2384=EDGE_LOOP('',(#7796,#7797,#7798));
#2385=EDGE_LOOP('',(#7799,#7800,#7801,#7802,#7803,#7804,#7805,#7806));
#2386=EDGE_LOOP('',(#7807,#7808,#7809,#7810,#7811,#7812,#7813,#7814,#7815,
#7816,#7817,#7818));
#2387=EDGE_LOOP('',(#7819));
#2388=EDGE_LOOP('',(#7820,#7821,#7822,#7823,#7824));
#2389=EDGE_LOOP('',(#7825,#7826,#7827,#7828));
#2390=EDGE_LOOP('',(#7829));
#2391=EDGE_LOOP('',(#7830));
#2392=EDGE_LOOP('',(#7831));
#2393=EDGE_LOOP('',(#7832));
#2394=EDGE_LOOP('',(#7833,#7834,#7835,#7836));
#2395=EDGE_LOOP('',(#7837));
#2396=EDGE_LOOP('',(#7838));
#2397=EDGE_LOOP('',(#7839,#7840,#7841,#7842));
#2398=EDGE_LOOP('',(#7843));
#2399=EDGE_LOOP('',(#7844));
#2400=EDGE_LOOP('',(#7845,#7846,#7847,#7848));
#2401=EDGE_LOOP('',(#7849));
#2402=EDGE_LOOP('',(#7850));
#2403=EDGE_LOOP('',(#7851,#7852,#7853,#7854));
#2404=EDGE_LOOP('',(#7855));
#2405=EDGE_LOOP('',(#7856));
#2406=EDGE_LOOP('',(#7857,#7858,#7859,#7860));
#2407=EDGE_LOOP('',(#7861));
#2408=EDGE_LOOP('',(#7862));
#2409=EDGE_LOOP('',(#7863,#7864,#7865,#7866));
#2410=EDGE_LOOP('',(#7867,#7868,#7869,#7870));
#2411=EDGE_LOOP('',(#7871,#7872,#7873,#7874));
#2412=EDGE_LOOP('',(#7875,#7876,#7877,#7878));
#2413=EDGE_LOOP('',(#7879,#7880,#7881,#7882));
#2414=EDGE_LOOP('',(#7883,#7884,#7885,#7886));
#2415=EDGE_LOOP('',(#7887));
#2416=EDGE_LOOP('',(#7888));
#2417=EDGE_LOOP('',(#7889));
#2418=EDGE_LOOP('',(#7890));
#2419=EDGE_LOOP('',(#7891,#7892,#7893,#7894));
#2420=EDGE_LOOP('',(#7895,#7896,#7897,#7898));
#2421=EDGE_LOOP('',(#7899));
#2422=EDGE_LOOP('',(#7900));
#2423=EDGE_LOOP('',(#7901));
#2424=EDGE_LOOP('',(#7902));
#2425=EDGE_LOOP('',(#7903,#7904,#7905,#7906));
#2426=EDGE_LOOP('',(#7907,#7908,#7909,#7910));
#2427=EDGE_LOOP('',(#7911,#7912,#7913,#7914));
#2428=EDGE_LOOP('',(#7915,#7916,#7917,#7918));
#2429=EDGE_LOOP('',(#7919,#7920,#7921,#7922));
#2430=EDGE_LOOP('',(#7923,#7924,#7925,#7926));
#2431=EDGE_LOOP('',(#7927,#7928,#7929,#7930));
#2432=EDGE_LOOP('',(#7931));
#2433=EDGE_LOOP('',(#7932));
#2434=EDGE_LOOP('',(#7933,#7934,#7935,#7936));
#2435=EDGE_LOOP('',(#7937));
#2436=EDGE_LOOP('',(#7938));
#2437=EDGE_LOOP('',(#7939,#7940,#7941,#7942));
#2438=EDGE_LOOP('',(#7943));
#2439=EDGE_LOOP('',(#7944));
#2440=EDGE_LOOP('',(#7945,#7946,#7947,#7948));
#2441=EDGE_LOOP('',(#7949));
#2442=EDGE_LOOP('',(#7950));
#2443=EDGE_LOOP('',(#7951,#7952,#7953,#7954));
#2444=EDGE_LOOP('',(#7955));
#2445=EDGE_LOOP('',(#7956));
#2446=EDGE_LOOP('',(#7957,#7958,#7959,#7960));
#2447=EDGE_LOOP('',(#7961));
#2448=EDGE_LOOP('',(#7962));
#2449=EDGE_LOOP('',(#7963,#7964,#7965,#7966));
#2450=EDGE_LOOP('',(#7967,#7968,#7969,#7970));
#2451=EDGE_LOOP('',(#7971,#7972,#7973,#7974));
#2452=EDGE_LOOP('',(#7975,#7976,#7977,#7978));
#2453=EDGE_LOOP('',(#7979,#7980,#7981,#7982));
#2454=EDGE_LOOP('',(#7983,#7984,#7985,#7986));
#2455=EDGE_LOOP('',(#7987));
#2456=EDGE_LOOP('',(#7988));
#2457=EDGE_LOOP('',(#7989,#7990,#7991,#7992));
#2458=EDGE_LOOP('',(#7993,#7994,#7995,#7996));
#2459=EDGE_LOOP('',(#7997));
#2460=EDGE_LOOP('',(#7998));
#2461=EDGE_LOOP('',(#7999,#8000,#8001,#8002));
#2462=EDGE_LOOP('',(#8003,#8004,#8005,#8006));
#2463=EDGE_LOOP('',(#8007,#8008,#8009,#8010));
#2464=EDGE_LOOP('',(#8011,#8012,#8013,#8014));
#2465=EDGE_LOOP('',(#8015,#8016,#8017,#8018));
#2466=EDGE_LOOP('',(#8019,#8020,#8021,#8022));
#2467=EDGE_LOOP('',(#8023,#8024,#8025,#8026));
#2468=EDGE_LOOP('',(#8027,#8028,#8029,#8030));
#2469=EDGE_LOOP('',(#8031,#8032,#8033,#8034,#8035,#8036));
#2470=EDGE_LOOP('',(#8037,#8038,#8039,#8040,#8041,#8042));
#2471=EDGE_LOOP('',(#8043));
#2472=EDGE_LOOP('',(#8044));
#2473=EDGE_LOOP('',(#8045,#8046,#8047,#8048));
#2474=EDGE_LOOP('',(#8049,#8050,#8051,#8052));
#2475=EDGE_LOOP('',(#8053,#8054,#8055,#8056));
#2476=EDGE_LOOP('',(#8057));
#2477=EDGE_LOOP('',(#8058));
#2478=EDGE_LOOP('',(#8059,#8060,#8061,#8062));
#2479=EDGE_LOOP('',(#8063,#8064,#8065,#8066));
#2480=EDGE_LOOP('',(#8067,#8068,#8069,#8070));
#2481=EDGE_LOOP('',(#8071));
#2482=EDGE_LOOP('',(#8072,#8073,#8074,#8075));
#2483=EDGE_LOOP('',(#8076));
#2484=EDGE_LOOP('',(#8077));
#2485=EDGE_LOOP('',(#8078));
#2486=EDGE_LOOP('',(#8079));
#2487=EDGE_LOOP('',(#8080));
#2488=EDGE_LOOP('',(#8081,#8082,#8083,#8084));
#2489=EDGE_LOOP('',(#8085,#8086,#8087,#8088));
#2490=EDGE_LOOP('',(#8089));
#2491=EDGE_LOOP('',(#8090));
#2492=EDGE_LOOP('',(#8091));
#2493=EDGE_LOOP('',(#8092));
#2494=EDGE_LOOP('',(#8093,#8094,#8095,#8096));
#2495=EDGE_LOOP('',(#8097,#8098,#8099,#8100));
#2496=EDGE_LOOP('',(#8101,#8102,#8103,#8104));
#2497=EDGE_LOOP('',(#8105));
#2498=EDGE_LOOP('',(#8106));
#2499=EDGE_LOOP('',(#8107));
#2500=EDGE_LOOP('',(#8108));
#2501=EDGE_LOOP('',(#8109,#8110,#8111,#8112));
#2502=EDGE_LOOP('',(#8113,#8114,#8115,#8116));
#2503=EDGE_LOOP('',(#8117));
#2504=EDGE_LOOP('',(#8118));
#2505=EDGE_LOOP('',(#8119));
#2506=EDGE_LOOP('',(#8120));
#2507=EDGE_LOOP('',(#8121,#8122,#8123,#8124));
#2508=EDGE_LOOP('',(#8125,#8126,#8127,#8128));
#2509=EDGE_LOOP('',(#8129));
#2510=EDGE_LOOP('',(#8130));
#2511=EDGE_LOOP('',(#8131));
#2512=EDGE_LOOP('',(#8132));
#2513=EDGE_LOOP('',(#8133,#8134,#8135,#8136));
#2514=EDGE_LOOP('',(#8137,#8138));
#2515=EDGE_LOOP('',(#8139,#8140,#8141,#8142,#8143,#8144,#8145,#8146,#8147,
#8148,#8149));
#2516=EDGE_LOOP('',(#8150,#8151));
#2517=EDGE_LOOP('',(#8152));
#2518=EDGE_LOOP('',(#8153));
#2519=EDGE_LOOP('',(#8154,#8155,#8156,#8157,#8158,#8159,#8160,#8161,#8162,
#8163,#8164,#8165));
#2520=EDGE_LOOP('',(#8166,#8167,#8168,#8169,#8170,#8171,#8172,#8173,#8174));
#2521=EDGE_LOOP('',(#8175));
#2522=EDGE_LOOP('',(#8176));
#2523=EDGE_LOOP('',(#8177));
#2524=EDGE_LOOP('',(#8178));
#2525=EDGE_LOOP('',(#8179,#8180,#8181,#8182));
#2526=EDGE_LOOP('',(#8183,#8184,#8185,#8186));
#2527=EDGE_LOOP('',(#8187));
#2528=EDGE_LOOP('',(#8188));
#2529=EDGE_LOOP('',(#8189));
#2530=EDGE_LOOP('',(#8190));
#2531=EDGE_LOOP('',(#8191,#8192,#8193,#8194));
#2532=EDGE_LOOP('',(#8195,#8196,#8197,#8198));
#2533=EDGE_LOOP('',(#8199));
#2534=EDGE_LOOP('',(#8200));
#2535=EDGE_LOOP('',(#8201));
#2536=EDGE_LOOP('',(#8202));
#2537=EDGE_LOOP('',(#8203,#8204));
#2538=EDGE_LOOP('',(#8205,#8206,#8207,#8208,#8209,#8210,#8211,#8212,#8213,
#8214,#8215));
#2539=EDGE_LOOP('',(#8216,#8217));
#2540=EDGE_LOOP('',(#8218,#8219,#8220,#8221,#8222,#8223,#8224,#8225,#8226,
#8227,#8228,#8229));
#2541=EDGE_LOOP('',(#8230,#8231,#8232,#8233,#8234,#8235,#8236,#8237,#8238));
#2542=EDGE_LOOP('',(#8239));
#2543=EDGE_LOOP('',(#8240));
#2544=EDGE_LOOP('',(#8241));
#2545=EDGE_LOOP('',(#8242));
#2546=EDGE_LOOP('',(#8243));
#2547=EDGE_LOOP('',(#8244,#8245,#8246,#8247));
#2548=EDGE_LOOP('',(#8248,#8249,#8250,#8251));
#2549=EDGE_LOOP('',(#8252,#8253,#8254,#8255));
#2550=EDGE_LOOP('',(#8256));
#2551=EDGE_LOOP('',(#8257));
#2552=EDGE_LOOP('',(#8258,#8259,#8260,#8261));
#2553=EDGE_LOOP('',(#8262,#8263,#8264,#8265));
#2554=EDGE_LOOP('',(#8266,#8267,#8268,#8269));
#2555=EDGE_LOOP('',(#8270));
#2556=EDGE_LOOP('',(#8271,#8272,#8273,#8274));
#2557=EDGE_LOOP('',(#8275,#8276,#8277,#8278));
#2558=EDGE_LOOP('',(#8279,#8280,#8281,#8282));
#2559=EDGE_LOOP('',(#8283,#8284,#8285,#8286));
#2560=EDGE_LOOP('',(#8287,#8288,#8289,#8290));
#2561=EDGE_LOOP('',(#8291,#8292,#8293,#8294));
#2562=EDGE_LOOP('',(#8295,#8296,#8297,#8298,#8299,#8300));
#2563=EDGE_LOOP('',(#8301,#8302,#8303,#8304,#8305,#8306));
#2564=EDGE_LOOP('',(#8307,#8308,#8309,#8310));
#2565=EDGE_LOOP('',(#8311,#8312,#8313,#8314));
#2566=EDGE_LOOP('',(#8315,#8316,#8317,#8318));
#2567=EDGE_LOOP('',(#8319,#8320,#8321,#8322));
#2568=EDGE_LOOP('',(#8323,#8324,#8325,#8326));
#2569=EDGE_LOOP('',(#8327,#8328,#8329,#8330));
#2570=EDGE_LOOP('',(#8331,#8332,#8333,#8334,#8335,#8336));
#2571=EDGE_LOOP('',(#8337));
#2572=EDGE_LOOP('',(#8338,#8339,#8340,#8341,#8342,#8343));
#2573=EDGE_LOOP('',(#8344,#8345,#8346,#8347));
#2574=EDGE_LOOP('',(#8348,#8349,#8350,#8351));
#2575=EDGE_LOOP('',(#8352,#8353,#8354,#8355));
#2576=EDGE_LOOP('',(#8356));
#2577=LINE('',#13682,#3150);
#2578=LINE('',#13688,#3151);
#2579=LINE('',#13694,#3152);
#2580=LINE('',#13700,#3153);
#2581=LINE('',#13706,#3154);
#2582=LINE('',#13712,#3155);
#2583=LINE('',#13718,#3156);
#2584=LINE('',#13724,#3157);
#2585=LINE('',#13730,#3158);
#2586=LINE('',#13736,#3159);
#2587=LINE('',#13742,#3160);
#2588=LINE('',#13748,#3161);
#2589=LINE('',#13753,#3162);
#2590=LINE('',#13755,#3163);
#2591=LINE('',#13757,#3164);
#2592=LINE('',#13758,#3165);
#2593=LINE('',#13761,#3166);
#2594=LINE('',#13763,#3167);
#2595=LINE('',#13764,#3168);
#2596=LINE('',#13767,#3169);
#2597=LINE('',#13769,#3170);
#2598=LINE('',#13770,#3171);
#2599=LINE('',#13772,#3172);
#2600=LINE('',#13773,#3173);
#2601=LINE('',#13780,#3174);
#2602=LINE('',#13782,#3175);
#2603=LINE('',#13784,#3176);
#2604=LINE('',#13785,#3177);
#2605=LINE('',#13788,#3178);
#2606=LINE('',#13790,#3179);
#2607=LINE('',#13791,#3180);
#2608=LINE('',#13794,#3181);
#2609=LINE('',#13796,#3182);
#2610=LINE('',#13797,#3183);
#2611=LINE('',#13799,#3184);
#2612=LINE('',#13800,#3185);
#2613=LINE('',#13807,#3186);
#2614=LINE('',#13809,#3187);
#2615=LINE('',#13811,#3188);
#2616=LINE('',#13812,#3189);
#2617=LINE('',#13815,#3190);
#2618=LINE('',#13817,#3191);
#2619=LINE('',#13818,#3192);
#2620=LINE('',#13821,#3193);
#2621=LINE('',#13823,#3194);
#2622=LINE('',#13824,#3195);
#2623=LINE('',#13826,#3196);
#2624=LINE('',#13827,#3197);
#2625=LINE('',#13834,#3198);
#2626=LINE('',#13838,#3199);
#2627=LINE('',#13843,#3200);
#2628=LINE('',#13847,#3201);
#2629=LINE('',#13852,#3202);
#2630=LINE('',#13885,#3203);
#2631=LINE('',#13888,#3204);
#2632=LINE('',#13891,#3205);
#2633=LINE('',#13898,#3206);
#2634=LINE('',#13906,#3207);
#2635=LINE('',#13907,#3208);
#2636=LINE('',#13909,#3209);
#2637=LINE('',#13911,#3210);
#2638=LINE('',#13912,#3211);
#2639=LINE('',#13913,#3212);
#2640=LINE('',#13917,#3213);
#2641=LINE('',#13921,#3214);
#2642=LINE('',#13925,#3215);
#2643=LINE('',#13927,#3216);
#2644=LINE('',#13932,#3217);
#2645=LINE('',#13933,#3218);
#2646=LINE('',#13934,#3219);
#2647=LINE('',#13937,#3220);
#2648=LINE('',#13938,#3221);
#2649=LINE('',#13941,#3222);
#2650=LINE('',#13942,#3223);
#2651=LINE('',#13944,#3224);
#2652=LINE('',#13950,#3225);
#2653=LINE('',#13954,#3226);
#2654=LINE('',#13959,#3227);
#2655=LINE('',#13963,#3228);
#2656=LINE('',#13968,#3229);
#2657=LINE('',#14001,#3230);
#2658=LINE('',#14004,#3231);
#2659=LINE('',#14007,#3232);
#2660=LINE('',#14014,#3233);
#2661=LINE('',#14022,#3234);
#2662=LINE('',#14023,#3235);
#2663=LINE('',#14025,#3236);
#2664=LINE('',#14027,#3237);
#2665=LINE('',#14028,#3238);
#2666=LINE('',#14029,#3239);
#2667=LINE('',#14033,#3240);
#2668=LINE('',#14037,#3241);
#2669=LINE('',#14041,#3242);
#2670=LINE('',#14043,#3243);
#2671=LINE('',#14048,#3244);
#2672=LINE('',#14049,#3245);
#2673=LINE('',#14050,#3246);
#2674=LINE('',#14053,#3247);
#2675=LINE('',#14054,#3248);
#2676=LINE('',#14057,#3249);
#2677=LINE('',#14058,#3250);
#2678=LINE('',#14060,#3251);
#2679=LINE('',#14066,#3252);
#2680=LINE('',#14070,#3253);
#2681=LINE('',#14075,#3254);
#2682=LINE('',#14079,#3255);
#2683=LINE('',#14084,#3256);
#2684=LINE('',#14117,#3257);
#2685=LINE('',#14120,#3258);
#2686=LINE('',#14123,#3259);
#2687=LINE('',#14130,#3260);
#2688=LINE('',#14138,#3261);
#2689=LINE('',#14139,#3262);
#2690=LINE('',#14141,#3263);
#2691=LINE('',#14143,#3264);
#2692=LINE('',#14144,#3265);
#2693=LINE('',#14145,#3266);
#2694=LINE('',#14149,#3267);
#2695=LINE('',#14153,#3268);
#2696=LINE('',#14157,#3269);
#2697=LINE('',#14159,#3270);
#2698=LINE('',#14164,#3271);
#2699=LINE('',#14165,#3272);
#2700=LINE('',#14166,#3273);
#2701=LINE('',#14169,#3274);
#2702=LINE('',#14170,#3275);
#2703=LINE('',#14173,#3276);
#2704=LINE('',#14174,#3277);
#2705=LINE('',#14176,#3278);
#2706=LINE('',#14182,#3279);
#2707=LINE('',#14186,#3280);
#2708=LINE('',#14191,#3281);
#2709=LINE('',#14195,#3282);
#2710=LINE('',#14200,#3283);
#2711=LINE('',#14233,#3284);
#2712=LINE('',#14236,#3285);
#2713=LINE('',#14239,#3286);
#2714=LINE('',#14246,#3287);
#2715=LINE('',#14254,#3288);
#2716=LINE('',#14255,#3289);
#2717=LINE('',#14257,#3290);
#2718=LINE('',#14259,#3291);
#2719=LINE('',#14260,#3292);
#2720=LINE('',#14261,#3293);
#2721=LINE('',#14265,#3294);
#2722=LINE('',#14269,#3295);
#2723=LINE('',#14273,#3296);
#2724=LINE('',#14275,#3297);
#2725=LINE('',#14280,#3298);
#2726=LINE('',#14281,#3299);
#2727=LINE('',#14282,#3300);
#2728=LINE('',#14285,#3301);
#2729=LINE('',#14286,#3302);
#2730=LINE('',#14289,#3303);
#2731=LINE('',#14290,#3304);
#2732=LINE('',#14292,#3305);
#2733=LINE('',#14299,#3306);
#2734=LINE('',#14305,#3307);
#2735=LINE('',#14311,#3308);
#2736=LINE('',#14317,#3309);
#2737=LINE('',#14323,#3310);
#2738=LINE('',#14329,#3311);
#2739=LINE('',#14335,#3312);
#2740=LINE('',#14340,#3313);
#2741=LINE('',#14342,#3314);
#2742=LINE('',#14344,#3315);
#2743=LINE('',#14345,#3316);
#2744=LINE('',#14349,#3317);
#2745=LINE('',#14351,#3318);
#2746=LINE('',#14353,#3319);
#2747=LINE('',#14354,#3320);
#2748=LINE('',#14357,#3321);
#2749=LINE('',#14359,#3322);
#2750=LINE('',#14360,#3323);
#2751=LINE('',#14363,#3324);
#2752=LINE('',#14365,#3325);
#2753=LINE('',#14366,#3326);
#2754=LINE('',#14369,#3327);
#2755=LINE('',#14371,#3328);
#2756=LINE('',#14372,#3329);
#2757=LINE('',#14375,#3330);
#2758=LINE('',#14376,#3331);
#2759=LINE('',#14377,#3332);
#2760=LINE('',#14380,#3333);
#2761=LINE('',#14381,#3334);
#2762=LINE('',#14383,#3335);
#2763=LINE('',#14384,#3336);
#2764=LINE('',#14392,#3337);
#2765=LINE('',#14398,#3338);
#2766=LINE('',#14404,#3339);
#2767=LINE('',#14410,#3340);
#2768=LINE('',#14416,#3341);
#2769=LINE('',#14423,#3342);
#2770=LINE('',#14429,#3343);
#2771=LINE('',#14438,#3344);
#2772=LINE('',#14444,#3345);
#2773=LINE('',#14450,#3346);
#2774=LINE('',#14456,#3347);
#2775=LINE('',#14462,#3348);
#2776=LINE('',#14470,#3349);
#2777=LINE('',#14475,#3350);
#2778=LINE('',#14484,#3351);
#2779=LINE('',#14490,#3352);
#2780=LINE('',#14496,#3353);
#2781=LINE('',#14502,#3354);
#2782=LINE('',#14508,#3355);
#2783=LINE('',#14514,#3356);
#2784=LINE('',#14520,#3357);
#2785=LINE('',#14525,#3358);
#2786=LINE('',#14527,#3359);
#2787=LINE('',#14529,#3360);
#2788=LINE('',#14530,#3361);
#2789=LINE('',#14534,#3362);
#2790=LINE('',#14536,#3363);
#2791=LINE('',#14538,#3364);
#2792=LINE('',#14539,#3365);
#2793=LINE('',#14542,#3366);
#2794=LINE('',#14544,#3367);
#2795=LINE('',#14545,#3368);
#2796=LINE('',#14548,#3369);
#2797=LINE('',#14550,#3370);
#2798=LINE('',#14551,#3371);
#2799=LINE('',#14554,#3372);
#2800=LINE('',#14556,#3373);
#2801=LINE('',#14557,#3374);
#2802=LINE('',#14560,#3375);
#2803=LINE('',#14561,#3376);
#2804=LINE('',#14562,#3377);
#2805=LINE('',#14565,#3378);
#2806=LINE('',#14566,#3379);
#2807=LINE('',#14568,#3380);
#2808=LINE('',#14569,#3381);
#2809=LINE('',#14577,#3382);
#2810=LINE('',#14583,#3383);
#2811=LINE('',#14589,#3384);
#2812=LINE('',#14595,#3385);
#2813=LINE('',#14601,#3386);
#2814=LINE('',#14608,#3387);
#2815=LINE('',#14614,#3388);
#2816=LINE('',#14623,#3389);
#2817=LINE('',#14629,#3390);
#2818=LINE('',#14635,#3391);
#2819=LINE('',#14641,#3392);
#2820=LINE('',#14647,#3393);
#2821=LINE('',#14655,#3394);
#2822=LINE('',#14660,#3395);
#2823=LINE('',#14669,#3396);
#2824=LINE('',#14674,#3397);
#2825=LINE('',#14679,#3398);
#2826=LINE('',#14695,#3399);
#2827=LINE('',#14701,#3400);
#2828=LINE('',#14705,#3401);
#2829=LINE('',#14711,#3402);
#2830=LINE('',#14716,#3403);
#2831=LINE('',#14731,#3404);
#2832=LINE('',#14740,#3405);
#2833=LINE('',#14744,#3406);
#2834=LINE('',#14748,#3407);
#2835=LINE('',#14751,#3408);
#2836=LINE('',#14887,#3409);
#2837=LINE('',#15140,#3410);
#2838=LINE('',#15182,#3411);
#2839=LINE('',#15187,#3412);
#2840=LINE('',#15196,#3413);
#2841=LINE('',#15201,#3414);
#2842=LINE('',#15213,#3415);
#2843=LINE('',#15220,#3416);
#2844=LINE('',#15227,#3417);
#2845=LINE('',#15234,#3418);
#2846=LINE('',#15241,#3419);
#2847=LINE('',#15248,#3420);
#2848=LINE('',#15255,#3421);
#2849=LINE('',#15261,#3422);
#2850=LINE('',#15267,#3423);
#2851=LINE('',#15273,#3424);
#2852=LINE('',#15279,#3425);
#2853=LINE('',#15285,#3426);
#2854=LINE('',#15291,#3427);
#2855=LINE('',#15296,#3428);
#2856=LINE('',#15298,#3429);
#2857=LINE('',#15300,#3430);
#2858=LINE('',#15301,#3431);
#2859=LINE('',#15304,#3432);
#2860=LINE('',#15306,#3433);
#2861=LINE('',#15307,#3434);
#2862=LINE('',#15310,#3435);
#2863=LINE('',#15312,#3436);
#2864=LINE('',#15313,#3437);
#2865=LINE('',#15315,#3438);
#2866=LINE('',#15316,#3439);
#2867=LINE('',#15324,#3440);
#2868=LINE('',#15330,#3441);
#2869=LINE('',#15336,#3442);
#2870=LINE('',#15342,#3443);
#2871=LINE('',#15348,#3444);
#2872=LINE('',#15354,#3445);
#2873=LINE('',#15360,#3446);
#2874=LINE('',#15365,#3447);
#2875=LINE('',#15367,#3448);
#2876=LINE('',#15369,#3449);
#2877=LINE('',#15370,#3450);
#2878=LINE('',#15373,#3451);
#2879=LINE('',#15375,#3452);
#2880=LINE('',#15376,#3453);
#2881=LINE('',#15379,#3454);
#2882=LINE('',#15381,#3455);
#2883=LINE('',#15382,#3456);
#2884=LINE('',#15384,#3457);
#2885=LINE('',#15385,#3458);
#2886=LINE('',#15393,#3459);
#2887=LINE('',#15399,#3460);
#2888=LINE('',#15405,#3461);
#2889=LINE('',#15411,#3462);
#2890=LINE('',#15417,#3463);
#2891=LINE('',#15423,#3464);
#2892=LINE('',#15429,#3465);
#2893=LINE('',#15434,#3466);
#2894=LINE('',#15436,#3467);
#2895=LINE('',#15438,#3468);
#2896=LINE('',#15439,#3469);
#2897=LINE('',#15442,#3470);
#2898=LINE('',#15444,#3471);
#2899=LINE('',#15445,#3472);
#2900=LINE('',#15448,#3473);
#2901=LINE('',#15450,#3474);
#2902=LINE('',#15451,#3475);
#2903=LINE('',#15453,#3476);
#2904=LINE('',#15454,#3477);
#2905=LINE('',#15467,#3478);
#2906=LINE('',#15470,#3479);
#2907=LINE('',#15472,#3480);
#2908=LINE('',#15483,#3481);
#2909=LINE('',#15487,#3482);
#2910=LINE('',#15491,#3483);
#2911=LINE('',#15495,#3484);
#2912=LINE('',#15504,#3485);
#2913=LINE('',#15510,#3486);
#2914=LINE('',#15518,#3487);
#2915=LINE('',#15527,#3488);
#2916=LINE('',#15536,#3489);
#2917=LINE('',#15545,#3490);
#2918=LINE('',#15553,#3491);
#2919=LINE('',#15557,#3492);
#2920=LINE('',#15561,#3493);
#2921=LINE('',#15565,#3494);
#2922=LINE('',#15569,#3495);
#2923=LINE('',#15571,#3496);
#2924=LINE('',#15573,#3497);
#2925=LINE('',#15574,#3498);
#2926=LINE('',#15577,#3499);
#2927=LINE('',#15579,#3500);
#2928=LINE('',#15580,#3501);
#2929=LINE('',#15583,#3502);
#2930=LINE('',#15585,#3503);
#2931=LINE('',#15586,#3504);
#2932=LINE('',#15588,#3505);
#2933=LINE('',#15589,#3506);
#2934=LINE('',#15598,#3507);
#2935=LINE('',#15605,#3508);
#2936=LINE('',#15612,#3509);
#2937=LINE('',#15619,#3510);
#2938=LINE('',#15626,#3511);
#2939=LINE('',#15633,#3512);
#2940=LINE('',#15640,#3513);
#2941=LINE('',#15646,#3514);
#2942=LINE('',#15652,#3515);
#2943=LINE('',#15658,#3516);
#2944=LINE('',#15664,#3517);
#2945=LINE('',#15670,#3518);
#2946=LINE('',#15676,#3519);
#2947=LINE('',#15681,#3520);
#2948=LINE('',#15683,#3521);
#2949=LINE('',#15685,#3522);
#2950=LINE('',#15686,#3523);
#2951=LINE('',#15689,#3524);
#2952=LINE('',#15691,#3525);
#2953=LINE('',#15692,#3526);
#2954=LINE('',#15695,#3527);
#2955=LINE('',#15697,#3528);
#2956=LINE('',#15698,#3529);
#2957=LINE('',#15700,#3530);
#2958=LINE('',#15701,#3531);
#2959=LINE('',#15709,#3532);
#2960=LINE('',#15715,#3533);
#2961=LINE('',#15721,#3534);
#2962=LINE('',#15727,#3535);
#2963=LINE('',#15733,#3536);
#2964=LINE('',#15739,#3537);
#2965=LINE('',#15745,#3538);
#2966=LINE('',#15750,#3539);
#2967=LINE('',#15752,#3540);
#2968=LINE('',#15754,#3541);
#2969=LINE('',#15755,#3542);
#2970=LINE('',#15758,#3543);
#2971=LINE('',#15760,#3544);
#2972=LINE('',#15761,#3545);
#2973=LINE('',#15764,#3546);
#2974=LINE('',#15766,#3547);
#2975=LINE('',#15767,#3548);
#2976=LINE('',#15769,#3549);
#2977=LINE('',#15770,#3550);
#2978=LINE('',#15778,#3551);
#2979=LINE('',#15784,#3552);
#2980=LINE('',#15790,#3553);
#2981=LINE('',#15796,#3554);
#2982=LINE('',#15802,#3555);
#2983=LINE('',#15808,#3556);
#2984=LINE('',#15814,#3557);
#2985=LINE('',#15819,#3558);
#2986=LINE('',#15821,#3559);
#2987=LINE('',#15823,#3560);
#2988=LINE('',#15824,#3561);
#2989=LINE('',#15827,#3562);
#2990=LINE('',#15829,#3563);
#2991=LINE('',#15830,#3564);
#2992=LINE('',#15833,#3565);
#2993=LINE('',#15835,#3566);
#2994=LINE('',#15836,#3567);
#2995=LINE('',#15838,#3568);
#2996=LINE('',#15839,#3569);
#2997=LINE('',#15853,#3570);
#2998=LINE('',#15855,#3571);
#2999=LINE('',#15858,#3572);
#3000=LINE('',#15870,#3573);
#3001=LINE('',#15873,#3574);
#3002=LINE('',#15875,#3575);
#3003=LINE('',#15880,#3576);
#3004=LINE('',#15888,#3577);
#3005=LINE('',#15896,#3578);
#3006=LINE('',#15903,#3579);
#3007=LINE('',#15912,#3580);
#3008=LINE('',#15921,#3581);
#3009=LINE('',#15930,#3582);
#3010=LINE('',#15937,#3583);
#3011=LINE('',#15941,#3584);
#3012=LINE('',#15945,#3585);
#3013=LINE('',#15949,#3586);
#3014=LINE('',#15954,#3587);
#3015=LINE('',#15956,#3588);
#3016=LINE('',#15958,#3589);
#3017=LINE('',#15959,#3590);
#3018=LINE('',#15962,#3591);
#3019=LINE('',#15964,#3592);
#3020=LINE('',#15965,#3593);
#3021=LINE('',#15968,#3594);
#3022=LINE('',#15970,#3595);
#3023=LINE('',#15971,#3596);
#3024=LINE('',#15973,#3597);
#3025=LINE('',#15974,#3598);
#3026=LINE('',#15984,#3599);
#3027=LINE('',#15986,#3600);
#3028=LINE('',#15987,#3601);
#3029=LINE('',#15990,#3602);
#3030=LINE('',#15992,#3603);
#3031=LINE('',#15993,#3604);
#3032=LINE('',#15998,#3605);
#3033=LINE('',#15999,#3606);
#3034=LINE('',#16001,#3607);
#3035=LINE('',#16002,#3608);
#3036=LINE('',#16012,#3609);
#3037=LINE('',#16019,#3610);
#3038=LINE('',#16026,#3611);
#3039=LINE('',#16033,#3612);
#3040=LINE('',#16040,#3613);
#3041=LINE('',#16045,#3614);
#3042=LINE('',#16052,#3615);
#3043=LINE('',#16055,#3616);
#3044=LINE('',#16058,#3617);
#3045=LINE('',#16060,#3618);
#3046=LINE('',#16061,#3619);
#3047=LINE('',#16067,#3620);
#3048=LINE('',#16069,#3621);
#3049=LINE('',#16070,#3622);
#3050=LINE('',#16079,#3623);
#3051=LINE('',#16084,#3624);
#3052=LINE('',#16091,#3625);
#3053=LINE('',#16093,#3626);
#3054=LINE('',#16095,#3627);
#3055=LINE('',#16096,#3628);
#3056=LINE('',#16099,#3629);
#3057=LINE('',#16101,#3630);
#3058=LINE('',#16102,#3631);
#3059=LINE('',#16105,#3632);
#3060=LINE('',#16107,#3633);
#3061=LINE('',#16108,#3634);
#3062=LINE('',#16111,#3635);
#3063=LINE('',#16113,#3636);
#3064=LINE('',#16114,#3637);
#3065=LINE('',#16117,#3638);
#3066=LINE('',#16119,#3639);
#3067=LINE('',#16120,#3640);
#3068=LINE('',#16122,#3641);
#3069=LINE('',#16123,#3642);
#3070=LINE('',#16135,#3643);
#3071=LINE('',#16139,#3644);
#3072=LINE('',#16143,#3645);
#3073=LINE('',#16150,#3646);
#3074=LINE('',#16152,#3647);
#3075=LINE('',#16159,#3648);
#3076=LINE('',#16166,#3649);
#3077=LINE('',#16180,#3650);
#3078=LINE('',#16183,#3651);
#3079=LINE('',#16194,#3652);
#3080=LINE('',#16197,#3653);
#3081=LINE('',#16202,#3654);
#3082=LINE('',#16210,#3655);
#3083=LINE('',#16216,#3656);
#3084=LINE('',#16225,#3657);
#3085=LINE('',#16231,#3658);
#3086=LINE('',#16240,#3659);
#3087=LINE('',#16245,#3660);
#3088=LINE('',#16278,#3661);
#3089=LINE('',#16320,#3662);
#3090=LINE('',#16327,#3663);
#3091=LINE('',#16329,#3664);
#3092=LINE('',#16334,#3665);
#3093=LINE('',#16335,#3666);
#3094=LINE('',#16343,#3667);
#3095=LINE('',#16349,#3668);
#3096=LINE('',#16358,#3669);
#3097=LINE('',#16364,#3670);
#3098=LINE('',#16372,#3671);
#3099=LINE('',#16413,#3672);
#3100=LINE('',#16455,#3673);
#3101=LINE('',#16459,#3674);
#3102=LINE('',#16461,#3675);
#3103=LINE('',#16466,#3676);
#3104=LINE('',#16468,#3677);
#3105=LINE('',#16479,#3678);
#3106=LINE('',#16483,#3679);
#3107=LINE('',#16487,#3680);
#3108=LINE('',#16494,#3681);
#3109=LINE('',#16498,#3682);
#3110=LINE('',#16502,#3683);
#3111=LINE('',#16507,#3684);
#3112=LINE('',#16509,#3685);
#3113=LINE('',#16511,#3686);
#3114=LINE('',#16512,#3687);
#3115=LINE('',#16515,#3688);
#3116=LINE('',#16517,#3689);
#3117=LINE('',#16518,#3690);
#3118=LINE('',#16521,#3691);
#3119=LINE('',#16523,#3692);
#3120=LINE('',#16524,#3693);
#3121=LINE('',#16527,#3694);
#3122=LINE('',#16529,#3695);
#3123=LINE('',#16530,#3696);
#3124=LINE('',#16533,#3697);
#3125=LINE('',#16535,#3698);
#3126=LINE('',#16536,#3699);
#3127=LINE('',#16538,#3700);
#3128=LINE('',#16539,#3701);
#3129=LINE('',#16588,#3702);
#3130=LINE('',#16590,#3703);
#3131=LINE('',#16592,#3704);
#3132=LINE('',#16593,#3705);
#3133=LINE('',#16596,#3706);
#3134=LINE('',#16598,#3707);
#3135=LINE('',#16599,#3708);
#3136=LINE('',#16602,#3709);
#3137=LINE('',#16604,#3710);
#3138=LINE('',#16605,#3711);
#3139=LINE('',#16608,#3712);
#3140=LINE('',#16610,#3713);
#3141=LINE('',#16611,#3714);
#3142=LINE('',#16614,#3715);
#3143=LINE('',#16616,#3716);
#3144=LINE('',#16617,#3717);
#3145=LINE('',#16619,#3718);
#3146=LINE('',#16620,#3719);
#3147=LINE('',#16628,#3720);
#3148=LINE('',#16632,#3721);
#3149=LINE('',#16636,#3722);
#3150=VECTOR('',#10762,0.164999999999999);
#3151=VECTOR('',#10769,0.164999999999999);
#3152=VECTOR('',#10776,0.164999999999999);
#3153=VECTOR('',#10783,0.164999999999999);
#3154=VECTOR('',#10790,0.164999999999999);
#3155=VECTOR('',#10797,0.164999999999999);
#3156=VECTOR('',#10804,0.164999999999999);
#3157=VECTOR('',#10811,0.164999999999999);
#3158=VECTOR('',#10818,0.164999999999999);
#3159=VECTOR('',#10825,0.164999999999999);
#3160=VECTOR('',#10832,0.164999999999999);
#3161=VECTOR('',#10839,0.164999999999999);
#3162=VECTOR('',#10844,1.);
#3163=VECTOR('',#10845,1.);
#3164=VECTOR('',#10846,1.);
#3165=VECTOR('',#10847,1.);
#3166=VECTOR('',#10850,1.);
#3167=VECTOR('',#10851,1.);
#3168=VECTOR('',#10852,1.);
#3169=VECTOR('',#10855,1.);
#3170=VECTOR('',#10856,1.);
#3171=VECTOR('',#10857,1.);
#3172=VECTOR('',#10860,1.);
#3173=VECTOR('',#10861,1.);
#3174=VECTOR('',#10870,1.);
#3175=VECTOR('',#10871,1.);
#3176=VECTOR('',#10872,1.);
#3177=VECTOR('',#10873,1.);
#3178=VECTOR('',#10876,1.);
#3179=VECTOR('',#10877,1.);
#3180=VECTOR('',#10878,1.);
#3181=VECTOR('',#10881,1.);
#3182=VECTOR('',#10882,1.);
#3183=VECTOR('',#10883,1.);
#3184=VECTOR('',#10886,1.);
#3185=VECTOR('',#10887,1.);
#3186=VECTOR('',#10896,1.);
#3187=VECTOR('',#10897,1.);
#3188=VECTOR('',#10898,1.);
#3189=VECTOR('',#10899,1.);
#3190=VECTOR('',#10902,1.);
#3191=VECTOR('',#10903,1.);
#3192=VECTOR('',#10904,1.);
#3193=VECTOR('',#10907,1.);
#3194=VECTOR('',#10908,1.);
#3195=VECTOR('',#10909,1.);
#3196=VECTOR('',#10912,1.);
#3197=VECTOR('',#10913,1.);
#3198=VECTOR('',#10922,0.4);
#3199=VECTOR('',#10925,1.);
#3200=VECTOR('',#10930,0.4);
#3201=VECTOR('',#10933,1.);
#3202=VECTOR('',#10938,1.);
#3203=VECTOR('',#10945,0.164999999999999);
#3204=VECTOR('',#10950,1.);
#3205=VECTOR('',#10955,1.);
#3206=VECTOR('',#10966,1.);
#3207=VECTOR('',#10975,1.);
#3208=VECTOR('',#10976,1.);
#3209=VECTOR('',#10977,1.);
#3210=VECTOR('',#10978,1.);
#3211=VECTOR('',#10979,1.);
#3212=VECTOR('',#10980,1.);
#3213=VECTOR('',#10985,0.225);
#3214=VECTOR('',#10990,0.225);
#3215=VECTOR('',#10995,0.6);
#3216=VECTOR('',#10996,0.6);
#3217=VECTOR('',#11001,1.);
#3218=VECTOR('',#11002,1.);
#3219=VECTOR('',#11003,1.);
#3220=VECTOR('',#11006,1.);
#3221=VECTOR('',#11007,1.);
#3222=VECTOR('',#11010,1.);
#3223=VECTOR('',#11011,1.);
#3224=VECTOR('',#11014,1.);
#3225=VECTOR('',#11021,0.4);
#3226=VECTOR('',#11024,1.);
#3227=VECTOR('',#11029,0.4);
#3228=VECTOR('',#11032,1.);
#3229=VECTOR('',#11037,1.);
#3230=VECTOR('',#11044,0.164999999999999);
#3231=VECTOR('',#11049,1.);
#3232=VECTOR('',#11054,1.);
#3233=VECTOR('',#11065,1.);
#3234=VECTOR('',#11074,1.);
#3235=VECTOR('',#11075,1.);
#3236=VECTOR('',#11076,1.);
#3237=VECTOR('',#11077,1.);
#3238=VECTOR('',#11078,1.);
#3239=VECTOR('',#11079,1.);
#3240=VECTOR('',#11084,0.225);
#3241=VECTOR('',#11089,0.225);
#3242=VECTOR('',#11094,0.6);
#3243=VECTOR('',#11095,0.6);
#3244=VECTOR('',#11100,1.);
#3245=VECTOR('',#11101,1.);
#3246=VECTOR('',#11102,1.);
#3247=VECTOR('',#11105,1.);
#3248=VECTOR('',#11106,1.);
#3249=VECTOR('',#11109,1.);
#3250=VECTOR('',#11110,1.);
#3251=VECTOR('',#11113,1.);
#3252=VECTOR('',#11120,0.4);
#3253=VECTOR('',#11123,1.);
#3254=VECTOR('',#11128,0.4);
#3255=VECTOR('',#11131,1.);
#3256=VECTOR('',#11136,1.);
#3257=VECTOR('',#11143,0.164999999999999);
#3258=VECTOR('',#11148,1.);
#3259=VECTOR('',#11153,1.);
#3260=VECTOR('',#11164,1.);
#3261=VECTOR('',#11173,1.);
#3262=VECTOR('',#11174,1.);
#3263=VECTOR('',#11175,1.);
#3264=VECTOR('',#11176,1.);
#3265=VECTOR('',#11177,1.);
#3266=VECTOR('',#11178,1.);
#3267=VECTOR('',#11183,0.225);
#3268=VECTOR('',#11188,0.225);
#3269=VECTOR('',#11193,0.6);
#3270=VECTOR('',#11194,0.6);
#3271=VECTOR('',#11199,1.);
#3272=VECTOR('',#11200,1.);
#3273=VECTOR('',#11201,1.);
#3274=VECTOR('',#11204,1.);
#3275=VECTOR('',#11205,1.);
#3276=VECTOR('',#11208,1.);
#3277=VECTOR('',#11209,1.);
#3278=VECTOR('',#11212,1.);
#3279=VECTOR('',#11219,0.4);
#3280=VECTOR('',#11222,1.);
#3281=VECTOR('',#11227,0.4);
#3282=VECTOR('',#11230,1.);
#3283=VECTOR('',#11235,1.);
#3284=VECTOR('',#11242,0.164999999999999);
#3285=VECTOR('',#11247,1.);
#3286=VECTOR('',#11252,1.);
#3287=VECTOR('',#11263,1.);
#3288=VECTOR('',#11272,1.);
#3289=VECTOR('',#11273,1.);
#3290=VECTOR('',#11274,1.);
#3291=VECTOR('',#11275,1.);
#3292=VECTOR('',#11276,1.);
#3293=VECTOR('',#11277,1.);
#3294=VECTOR('',#11282,0.225);
#3295=VECTOR('',#11287,0.225);
#3296=VECTOR('',#11292,0.6);
#3297=VECTOR('',#11293,0.6);
#3298=VECTOR('',#11298,1.);
#3299=VECTOR('',#11299,1.);
#3300=VECTOR('',#11300,1.);
#3301=VECTOR('',#11303,1.);
#3302=VECTOR('',#11304,1.);
#3303=VECTOR('',#11307,1.);
#3304=VECTOR('',#11308,1.);
#3305=VECTOR('',#11311,1.);
#3306=VECTOR('',#11320,0.165);
#3307=VECTOR('',#11327,0.165);
#3308=VECTOR('',#11334,0.165);
#3309=VECTOR('',#11341,0.165);
#3310=VECTOR('',#11348,0.225);
#3311=VECTOR('',#11355,0.225);
#3312=VECTOR('',#11362,1.6);
#3313=VECTOR('',#11367,1.);
#3314=VECTOR('',#11368,1.);
#3315=VECTOR('',#11369,1.);
#3316=VECTOR('',#11370,1.);
#3317=VECTOR('',#11373,1.);
#3318=VECTOR('',#11374,1.);
#3319=VECTOR('',#11375,1.);
#3320=VECTOR('',#11376,1.);
#3321=VECTOR('',#11379,1.);
#3322=VECTOR('',#11380,1.);
#3323=VECTOR('',#11381,1.);
#3324=VECTOR('',#11384,1.);
#3325=VECTOR('',#11385,1.);
#3326=VECTOR('',#11386,1.);
#3327=VECTOR('',#11389,1.);
#3328=VECTOR('',#11390,1.);
#3329=VECTOR('',#11391,1.);
#3330=VECTOR('',#11394,1.);
#3331=VECTOR('',#11395,1.);
#3332=VECTOR('',#11396,1.);
#3333=VECTOR('',#11399,1.);
#3334=VECTOR('',#11400,1.);
#3335=VECTOR('',#11403,1.);
#3336=VECTOR('',#11404,1.);
#3337=VECTOR('',#11415,0.225);
#3338=VECTOR('',#11422,0.225);
#3339=VECTOR('',#11429,0.225);
#3340=VECTOR('',#11436,0.225);
#3341=VECTOR('',#11443,1.59);
#3342=VECTOR('',#11452,1.005);
#3343=VECTOR('',#11459,2.4);
#3344=VECTOR('',#11472,0.225);
#3345=VECTOR('',#11479,0.225);
#3346=VECTOR('',#11486,0.225);
#3347=VECTOR('',#11493,0.225);
#3348=VECTOR('',#11500,1.59);
#3349=VECTOR('',#11511,1.005);
#3350=VECTOR('',#11516,2.4);
#3351=VECTOR('',#11529,0.165);
#3352=VECTOR('',#11536,0.165);
#3353=VECTOR('',#11543,0.165);
#3354=VECTOR('',#11550,0.165);
#3355=VECTOR('',#11557,0.225);
#3356=VECTOR('',#11564,0.225);
#3357=VECTOR('',#11571,1.6);
#3358=VECTOR('',#11576,1.);
#3359=VECTOR('',#11577,1.);
#3360=VECTOR('',#11578,1.);
#3361=VECTOR('',#11579,1.);
#3362=VECTOR('',#11582,1.);
#3363=VECTOR('',#11583,1.);
#3364=VECTOR('',#11584,1.);
#3365=VECTOR('',#11585,1.);
#3366=VECTOR('',#11588,1.);
#3367=VECTOR('',#11589,1.);
#3368=VECTOR('',#11590,1.);
#3369=VECTOR('',#11593,1.);
#3370=VECTOR('',#11594,1.);
#3371=VECTOR('',#11595,1.);
#3372=VECTOR('',#11598,1.);
#3373=VECTOR('',#11599,1.);
#3374=VECTOR('',#11600,1.);
#3375=VECTOR('',#11603,1.);
#3376=VECTOR('',#11604,1.);
#3377=VECTOR('',#11605,1.);
#3378=VECTOR('',#11608,1.);
#3379=VECTOR('',#11609,1.);
#3380=VECTOR('',#11612,1.);
#3381=VECTOR('',#11613,1.);
#3382=VECTOR('',#11624,0.225);
#3383=VECTOR('',#11631,0.225);
#3384=VECTOR('',#11638,0.225);
#3385=VECTOR('',#11645,0.225);
#3386=VECTOR('',#11652,1.59);
#3387=VECTOR('',#11661,1.005);
#3388=VECTOR('',#11668,2.4);
#3389=VECTOR('',#11681,0.225);
#3390=VECTOR('',#11688,0.225);
#3391=VECTOR('',#11695,0.225);
#3392=VECTOR('',#11702,0.225);
#3393=VECTOR('',#11709,1.59);
#3394=VECTOR('',#11720,1.005);
#3395=VECTOR('',#11725,2.4);
#3396=VECTOR('',#11738,0.55);
#3397=VECTOR('',#11745,0.6);
#3398=VECTOR('',#11752,0.55);
#3399=VECTOR('',#11773,1.070235);
#3400=VECTOR('',#11780,0.6);
#3401=VECTOR('',#11785,0.63);
#3402=VECTOR('',#11794,1.070235);
#3403=VECTOR('',#11801,0.63);
#3404=VECTOR('',#11820,1.129765);
#3405=VECTOR('',#11831,1.57);
#3406=VECTOR('',#11836,1.6);
#3407=VECTOR('',#11841,1.57);
#3408=VECTOR('',#11846,1.129765);
#3409=VECTOR('',#11893,1.123812);
#3410=VECTOR('',#11962,1.076188);
#3411=VECTOR('',#11991,1.119765);
#3412=VECTOR('',#11998,1.085235);
#3413=VECTOR('',#12009,1.119765);
#3414=VECTOR('',#12016,1.085235);
#3415=VECTOR('',#12035,0.165);
#3416=VECTOR('',#12044,0.164999999999999);
#3417=VECTOR('',#12053,0.165);
#3418=VECTOR('',#12062,0.164999999999999);
#3419=VECTOR('',#12071,0.165);
#3420=VECTOR('',#12080,0.165);
#3421=VECTOR('',#12089,0.165);
#3422=VECTOR('',#12096,0.165);
#3423=VECTOR('',#12103,0.165);
#3424=VECTOR('',#12110,0.165);
#3425=VECTOR('',#12117,1.1);
#3426=VECTOR('',#12124,1.05);
#3427=VECTOR('',#12131,1.05);
#3428=VECTOR('',#12136,1.);
#3429=VECTOR('',#12137,1.);
#3430=VECTOR('',#12138,1.);
#3431=VECTOR('',#12139,1.);
#3432=VECTOR('',#12142,1.);
#3433=VECTOR('',#12143,1.);
#3434=VECTOR('',#12144,1.);
#3435=VECTOR('',#12147,1.);
#3436=VECTOR('',#12148,1.);
#3437=VECTOR('',#12149,1.);
#3438=VECTOR('',#12152,1.);
#3439=VECTOR('',#12153,1.);
#3440=VECTOR('',#12164,0.225);
#3441=VECTOR('',#12171,0.225);
#3442=VECTOR('',#12178,0.225);
#3443=VECTOR('',#12185,0.225);
#3444=VECTOR('',#12192,1.65);
#3445=VECTOR('',#12199,0.7);
#3446=VECTOR('',#12206,0.7);
#3447=VECTOR('',#12211,1.);
#3448=VECTOR('',#12212,1.);
#3449=VECTOR('',#12213,1.);
#3450=VECTOR('',#12214,1.);
#3451=VECTOR('',#12217,1.);
#3452=VECTOR('',#12218,1.);
#3453=VECTOR('',#12219,1.);
#3454=VECTOR('',#12222,1.);
#3455=VECTOR('',#12223,1.);
#3456=VECTOR('',#12224,1.);
#3457=VECTOR('',#12227,1.);
#3458=VECTOR('',#12228,1.);
#3459=VECTOR('',#12239,0.225);
#3460=VECTOR('',#12246,0.225);
#3461=VECTOR('',#12253,0.225);
#3462=VECTOR('',#12260,0.225);
#3463=VECTOR('',#12267,1.65);
#3464=VECTOR('',#12274,0.7);
#3465=VECTOR('',#12281,0.7);
#3466=VECTOR('',#12286,1.);
#3467=VECTOR('',#12287,1.);
#3468=VECTOR('',#12288,1.);
#3469=VECTOR('',#12289,1.);
#3470=VECTOR('',#12292,1.);
#3471=VECTOR('',#12293,1.);
#3472=VECTOR('',#12294,1.);
#3473=VECTOR('',#12297,1.);
#3474=VECTOR('',#12298,1.);
#3475=VECTOR('',#12299,1.);
#3476=VECTOR('',#12302,1.);
#3477=VECTOR('',#12303,1.);
#3478=VECTOR('',#12320,1.);
#3479=VECTOR('',#12323,1.);
#3480=VECTOR('',#12324,0.225);
#3481=VECTOR('',#12337,1.);
#3482=VECTOR('',#12340,0.225);
#3483=VECTOR('',#12345,1.);
#3484=VECTOR('',#12350,1.1);
#3485=VECTOR('',#12363,1.6);
#3486=VECTOR('',#12370,0.525);
#3487=VECTOR('',#12381,0.4);
#3488=VECTOR('',#12392,0.4);
#3489=VECTOR('',#12403,0.4);
#3490=VECTOR('',#12414,0.4);
#3491=VECTOR('',#12425,0.225);
#3492=VECTOR('',#12430,0.225);
#3493=VECTOR('',#12435,0.225);
#3494=VECTOR('',#12440,0.225);
#3495=VECTOR('',#12443,1.);
#3496=VECTOR('',#12444,1.);
#3497=VECTOR('',#12445,1.);
#3498=VECTOR('',#12446,1.);
#3499=VECTOR('',#12449,1.);
#3500=VECTOR('',#12450,1.);
#3501=VECTOR('',#12451,1.);
#3502=VECTOR('',#12454,1.);
#3503=VECTOR('',#12455,1.);
#3504=VECTOR('',#12456,1.);
#3505=VECTOR('',#12459,1.);
#3506=VECTOR('',#12460,1.);
#3507=VECTOR('',#12473,0.165);
#3508=VECTOR('',#12482,0.164999999999999);
#3509=VECTOR('',#12491,0.165);
#3510=VECTOR('',#12500,0.164999999999999);
#3511=VECTOR('',#12509,0.165);
#3512=VECTOR('',#12518,0.165);
#3513=VECTOR('',#12527,0.165);
#3514=VECTOR('',#12534,0.165);
#3515=VECTOR('',#12541,0.165);
#3516=VECTOR('',#12548,0.165);
#3517=VECTOR('',#12555,1.1);
#3518=VECTOR('',#12562,1.05);
#3519=VECTOR('',#12569,1.05);
#3520=VECTOR('',#12574,1.);
#3521=VECTOR('',#12575,1.);
#3522=VECTOR('',#12576,1.);
#3523=VECTOR('',#12577,1.);
#3524=VECTOR('',#12580,1.);
#3525=VECTOR('',#12581,1.);
#3526=VECTOR('',#12582,1.);
#3527=VECTOR('',#12585,1.);
#3528=VECTOR('',#12586,1.);
#3529=VECTOR('',#12587,1.);
#3530=VECTOR('',#12590,1.);
#3531=VECTOR('',#12591,1.);
#3532=VECTOR('',#12602,0.225);
#3533=VECTOR('',#12609,0.225);
#3534=VECTOR('',#12616,0.225);
#3535=VECTOR('',#12623,0.225);
#3536=VECTOR('',#12630,1.65);
#3537=VECTOR('',#12637,0.7);
#3538=VECTOR('',#12644,0.7);
#3539=VECTOR('',#12649,1.);
#3540=VECTOR('',#12650,1.);
#3541=VECTOR('',#12651,1.);
#3542=VECTOR('',#12652,1.);
#3543=VECTOR('',#12655,1.);
#3544=VECTOR('',#12656,1.);
#3545=VECTOR('',#12657,1.);
#3546=VECTOR('',#12660,1.);
#3547=VECTOR('',#12661,1.);
#3548=VECTOR('',#12662,1.);
#3549=VECTOR('',#12665,1.);
#3550=VECTOR('',#12666,1.);
#3551=VECTOR('',#12677,0.225);
#3552=VECTOR('',#12684,0.225);
#3553=VECTOR('',#12691,0.225);
#3554=VECTOR('',#12698,0.225);
#3555=VECTOR('',#12705,1.65);
#3556=VECTOR('',#12712,0.7);
#3557=VECTOR('',#12719,0.7);
#3558=VECTOR('',#12724,1.);
#3559=VECTOR('',#12725,1.);
#3560=VECTOR('',#12726,1.);
#3561=VECTOR('',#12727,1.);
#3562=VECTOR('',#12730,1.);
#3563=VECTOR('',#12731,1.);
#3564=VECTOR('',#12732,1.);
#3565=VECTOR('',#12735,1.);
#3566=VECTOR('',#12736,1.);
#3567=VECTOR('',#12737,1.);
#3568=VECTOR('',#12740,1.);
#3569=VECTOR('',#12741,1.);
#3570=VECTOR('',#12760,0.225);
#3571=VECTOR('',#12761,1.);
#3572=VECTOR('',#12764,1.);
#3573=VECTOR('',#12777,0.225);
#3574=VECTOR('',#12780,1.);
#3575=VECTOR('',#12781,1.);
#3576=VECTOR('',#12788,1.1);
#3577=VECTOR('',#12799,1.6);
#3578=VECTOR('',#12810,0.525);
#3579=VECTOR('',#12819,0.4);
#3580=VECTOR('',#12830,0.4);
#3581=VECTOR('',#12841,0.4);
#3582=VECTOR('',#12852,0.4);
#3583=VECTOR('',#12861,0.225);
#3584=VECTOR('',#12866,0.225);
#3585=VECTOR('',#12871,0.225);
#3586=VECTOR('',#12876,0.225);
#3587=VECTOR('',#12881,1.);
#3588=VECTOR('',#12882,1.);
#3589=VECTOR('',#12883,1.);
#3590=VECTOR('',#12884,1.);
#3591=VECTOR('',#12887,1.);
#3592=VECTOR('',#12888,1.);
#3593=VECTOR('',#12889,1.);
#3594=VECTOR('',#12892,1.);
#3595=VECTOR('',#12893,1.);
#3596=VECTOR('',#12894,1.);
#3597=VECTOR('',#12897,1.);
#3598=VECTOR('',#12898,1.);
#3599=VECTOR('',#12911,1.);
#3600=VECTOR('',#12912,1.);
#3601=VECTOR('',#12913,1.);
#3602=VECTOR('',#12916,1.);
#3603=VECTOR('',#12917,1.);
#3604=VECTOR('',#12918,1.);
#3605=VECTOR('',#12923,1.);
#3606=VECTOR('',#12924,1.);
#3607=VECTOR('',#12927,1.);
#3608=VECTOR('',#12928,1.);
#3609=VECTOR('',#12941,1.05);
#3610=VECTOR('',#12950,1.);
#3611=VECTOR('',#12959,1.05);
#3612=VECTOR('',#12968,1.);
#3613=VECTOR('',#12977,1.05);
#3614=VECTOR('',#12984,0.9);
#3615=VECTOR('',#12991,1.);
#3616=VECTOR('',#12994,1.);
#3617=VECTOR('',#12997,1.);
#3618=VECTOR('',#12998,1.);
#3619=VECTOR('',#12999,1.);
#3620=VECTOR('',#13006,1.);
#3621=VECTOR('',#13009,1.);
#3622=VECTOR('',#13010,1.);
#3623=VECTOR('',#13021,0.895);
#3624=VECTOR('',#13028,0.605);
#3625=VECTOR('',#13037,1.);
#3626=VECTOR('',#13038,1.);
#3627=VECTOR('',#13039,1.);
#3628=VECTOR('',#13040,1.);
#3629=VECTOR('',#13043,1.);
#3630=VECTOR('',#13044,1.);
#3631=VECTOR('',#13045,1.);
#3632=VECTOR('',#13048,1.);
#3633=VECTOR('',#13049,1.);
#3634=VECTOR('',#13050,1.);
#3635=VECTOR('',#13053,1.);
#3636=VECTOR('',#13054,1.);
#3637=VECTOR('',#13055,1.);
#3638=VECTOR('',#13058,1.);
#3639=VECTOR('',#13059,1.);
#3640=VECTOR('',#13060,1.);
#3641=VECTOR('',#13063,1.);
#3642=VECTOR('',#13064,1.);
#3643=VECTOR('',#13081,0.325);
#3644=VECTOR('',#13086,0.35);
#3645=VECTOR('',#13091,0.335);
#3646=VECTOR('',#13100,0.21);
#3647=VECTOR('',#13103,0.2);
#3648=VECTOR('',#13112,0.165);
#3649=VECTOR('',#13121,0.165);
#3650=VECTOR('',#13140,0.8);
#3651=VECTOR('',#13143,0.6);
#3652=VECTOR('',#13158,0.8);
#3653=VECTOR('',#13161,0.6);
#3654=VECTOR('',#13168,0.6);
#3655=VECTOR('',#13179,0.605);
#3656=VECTOR('',#13186,0.8);
#3657=VECTOR('',#13199,0.605);
#3658=VECTOR('',#13206,0.8);
#3659=VECTOR('',#13219,2.3);
#3660=VECTOR('',#13224,1.);
#3661=VECTOR('',#13231,0.164999999999999);
#3662=VECTOR('',#13234,1.);
#3663=VECTOR('',#13243,0.6);
#3664=VECTOR('',#13244,0.6);
#3665=VECTOR('',#13251,1.2);
#3666=VECTOR('',#13252,1.2);
#3667=VECTOR('',#13263,0.225);
#3668=VECTOR('',#13270,1.);
#3669=VECTOR('',#13283,0.225);
#3670=VECTOR('',#13290,1.);
#3671=VECTOR('',#13301,1.);
#3672=VECTOR('',#13308,0.164999999999999);
#3673=VECTOR('',#13311,1.);
#3674=VECTOR('',#13316,0.605);
#3675=VECTOR('',#13317,0.605);
#3676=VECTOR('',#13324,1.);
#3677=VECTOR('',#13325,1.);
#3678=VECTOR('',#13342,0.325);
#3679=VECTOR('',#13347,0.35);
#3680=VECTOR('',#13352,0.335);
#3681=VECTOR('',#13361,0.21);
#3682=VECTOR('',#13366,0.2);
#3683=VECTOR('',#13371,0.18);
#3684=VECTOR('',#13376,1.);
#3685=VECTOR('',#13377,1.);
#3686=VECTOR('',#13378,1.);
#3687=VECTOR('',#13379,1.);
#3688=VECTOR('',#13382,1.);
#3689=VECTOR('',#13383,1.);
#3690=VECTOR('',#13384,1.);
#3691=VECTOR('',#13387,1.);
#3692=VECTOR('',#13388,1.);
#3693=VECTOR('',#13389,1.);
#3694=VECTOR('',#13392,1.);
#3695=VECTOR('',#13393,1.);
#3696=VECTOR('',#13394,1.);
#3697=VECTOR('',#13397,1.);
#3698=VECTOR('',#13398,1.);
#3699=VECTOR('',#13399,1.);
#3700=VECTOR('',#13402,1.);
#3701=VECTOR('',#13403,1.);
#3702=VECTOR('',#13496,1.);
#3703=VECTOR('',#13497,1.);
#3704=VECTOR('',#13498,1.);
#3705=VECTOR('',#13499,1.);
#3706=VECTOR('',#13502,1.);
#3707=VECTOR('',#13503,1.);
#3708=VECTOR('',#13504,1.);
#3709=VECTOR('',#13507,1.);
#3710=VECTOR('',#13508,1.);
#3711=VECTOR('',#13509,1.);
#3712=VECTOR('',#13512,1.);
#3713=VECTOR('',#13513,1.);
#3714=VECTOR('',#13514,1.);
#3715=VECTOR('',#13517,1.);
#3716=VECTOR('',#13518,1.);
#3717=VECTOR('',#13519,1.);
#3718=VECTOR('',#13522,1.);
#3719=VECTOR('',#13523,1.);
#3720=VECTOR('',#13534,0.185);
#3721=VECTOR('',#13539,0.2);
#3722=VECTOR('',#13544,0.1625);
#3723=CIRCLE('',#9581,0.164999999999999);
#3724=CIRCLE('',#9582,0.164999999999999);
#3725=CIRCLE('',#9584,0.164999999999999);
#3726=CIRCLE('',#9585,0.164999999999999);
#3727=CIRCLE('',#9587,0.164999999999999);
#3728=CIRCLE('',#9588,0.164999999999999);
#3729=CIRCLE('',#9590,0.164999999999999);
#3730=CIRCLE('',#9591,0.164999999999999);
#3731=CIRCLE('',#9593,0.164999999999999);
#3732=CIRCLE('',#9594,0.164999999999999);
#3733=CIRCLE('',#9596,0.164999999999999);
#3734=CIRCLE('',#9597,0.164999999999999);
#3735=CIRCLE('',#9599,0.164999999999999);
#3736=CIRCLE('',#9600,0.164999999999999);
#3737=CIRCLE('',#9602,0.164999999999999);
#3738=CIRCLE('',#9603,0.164999999999999);
#3739=CIRCLE('',#9605,0.164999999999999);
#3740=CIRCLE('',#9606,0.164999999999999);
#3741=CIRCLE('',#9608,0.164999999999999);
#3742=CIRCLE('',#9609,0.164999999999999);
#3743=CIRCLE('',#9611,0.164999999999999);
#3744=CIRCLE('',#9612,0.164999999999999);
#3745=CIRCLE('',#9614,0.164999999999999);
#3746=CIRCLE('',#9615,0.164999999999999);
#3747=CIRCLE('',#9638,0.4);
#3748=CIRCLE('',#9639,0.4);
#3749=CIRCLE('',#9641,0.4);
#3750=CIRCLE('',#9642,0.4);
#3751=CIRCLE('',#9644,0.164999999999999);
#3752=CIRCLE('',#9646,0.164999999999999);
#3753=CIRCLE('',#9647,0.164999999999999);
#3754=CIRCLE('',#9650,0.4);
#3755=CIRCLE('',#9651,0.4);
#3756=CIRCLE('',#9653,0.225);
#3757=CIRCLE('',#9655,0.4);
#3758=CIRCLE('',#9656,0.4);
#3759=CIRCLE('',#9658,0.225);
#3760=CIRCLE('',#9661,0.225);
#3761=CIRCLE('',#9663,0.225);
#3762=CIRCLE('',#9665,0.6);
#3763=CIRCLE('',#9666,0.6);
#3764=CIRCLE('',#9674,0.4);
#3765=CIRCLE('',#9675,0.4);
#3766=CIRCLE('',#9677,0.4);
#3767=CIRCLE('',#9678,0.4);
#3768=CIRCLE('',#9680,0.164999999999999);
#3769=CIRCLE('',#9682,0.164999999999999);
#3770=CIRCLE('',#9683,0.164999999999999);
#3771=CIRCLE('',#9686,0.4);
#3772=CIRCLE('',#9687,0.4);
#3773=CIRCLE('',#9689,0.225);
#3774=CIRCLE('',#9691,0.4);
#3775=CIRCLE('',#9692,0.4);
#3776=CIRCLE('',#9694,0.225);
#3777=CIRCLE('',#9697,0.225);
#3778=CIRCLE('',#9699,0.225);
#3779=CIRCLE('',#9701,0.6);
#3780=CIRCLE('',#9702,0.6);
#3781=CIRCLE('',#9710,0.4);
#3782=CIRCLE('',#9711,0.4);
#3783=CIRCLE('',#9713,0.4);
#3784=CIRCLE('',#9714,0.4);
#3785=CIRCLE('',#9716,0.164999999999999);
#3786=CIRCLE('',#9718,0.164999999999999);
#3787=CIRCLE('',#9719,0.164999999999999);
#3788=CIRCLE('',#9722,0.4);
#3789=CIRCLE('',#9723,0.4);
#3790=CIRCLE('',#9725,0.225);
#3791=CIRCLE('',#9727,0.4);
#3792=CIRCLE('',#9728,0.4);
#3793=CIRCLE('',#9730,0.225);
#3794=CIRCLE('',#9733,0.225);
#3795=CIRCLE('',#9735,0.225);
#3796=CIRCLE('',#9737,0.6);
#3797=CIRCLE('',#9738,0.6);
#3798=CIRCLE('',#9746,0.4);
#3799=CIRCLE('',#9747,0.4);
#3800=CIRCLE('',#9749,0.4);
#3801=CIRCLE('',#9750,0.4);
#3802=CIRCLE('',#9752,0.164999999999999);
#3803=CIRCLE('',#9754,0.164999999999999);
#3804=CIRCLE('',#9755,0.164999999999999);
#3805=CIRCLE('',#9758,0.4);
#3806=CIRCLE('',#9759,0.4);
#3807=CIRCLE('',#9761,0.225);
#3808=CIRCLE('',#9763,0.4);
#3809=CIRCLE('',#9764,0.4);
#3810=CIRCLE('',#9766,0.225);
#3811=CIRCLE('',#9769,0.225);
#3812=CIRCLE('',#9771,0.225);
#3813=CIRCLE('',#9773,0.6);
#3814=CIRCLE('',#9774,0.6);
#3815=CIRCLE('',#9782,0.165);
#3816=CIRCLE('',#9783,0.165);
#3817=CIRCLE('',#9785,0.165);
#3818=CIRCLE('',#9786,0.165);
#3819=CIRCLE('',#9788,0.165);
#3820=CIRCLE('',#9789,0.165);
#3821=CIRCLE('',#9791,0.165);
#3822=CIRCLE('',#9792,0.165);
#3823=CIRCLE('',#9794,0.225);
#3824=CIRCLE('',#9795,0.225);
#3825=CIRCLE('',#9797,0.225);
#3826=CIRCLE('',#9798,0.225);
#3827=CIRCLE('',#9800,1.6);
#3828=CIRCLE('',#9801,1.6);
#3829=CIRCLE('',#9814,0.225);
#3830=CIRCLE('',#9815,0.225);
#3831=CIRCLE('',#9817,0.225);
#3832=CIRCLE('',#9818,0.225);
#3833=CIRCLE('',#9820,0.225);
#3834=CIRCLE('',#9821,0.225);
#3835=CIRCLE('',#9823,0.225);
#3836=CIRCLE('',#9824,0.225);
#3837=CIRCLE('',#9826,1.59);
#3838=CIRCLE('',#9827,1.59);
#3839=CIRCLE('',#9829,1.005);
#3840=CIRCLE('',#9831,1.005);
#3841=CIRCLE('',#9833,2.4);
#3842=CIRCLE('',#9834,2.4);
#3843=CIRCLE('',#9839,0.225);
#3844=CIRCLE('',#9840,0.225);
#3845=CIRCLE('',#9842,0.225);
#3846=CIRCLE('',#9843,0.225);
#3847=CIRCLE('',#9845,0.225);
#3848=CIRCLE('',#9846,0.225);
#3849=CIRCLE('',#9848,0.225);
#3850=CIRCLE('',#9849,0.225);
#3851=CIRCLE('',#9851,1.59);
#3852=CIRCLE('',#9852,1.59);
#3853=CIRCLE('',#9854,1.005);
#3854=CIRCLE('',#9856,1.005);
#3855=CIRCLE('',#9858,2.4);
#3856=CIRCLE('',#9859,2.4);
#3857=CIRCLE('',#9864,0.165);
#3858=CIRCLE('',#9865,0.165);
#3859=CIRCLE('',#9867,0.165);
#3860=CIRCLE('',#9868,0.165);
#3861=CIRCLE('',#9870,0.165);
#3862=CIRCLE('',#9871,0.165);
#3863=CIRCLE('',#9873,0.165);
#3864=CIRCLE('',#9874,0.165);
#3865=CIRCLE('',#9876,0.225);
#3866=CIRCLE('',#9877,0.225);
#3867=CIRCLE('',#9879,0.225);
#3868=CIRCLE('',#9880,0.225);
#3869=CIRCLE('',#9882,1.6);
#3870=CIRCLE('',#9883,1.6);
#3871=CIRCLE('',#9896,0.225);
#3872=CIRCLE('',#9897,0.225);
#3873=CIRCLE('',#9899,0.225);
#3874=CIRCLE('',#9900,0.225);
#3875=CIRCLE('',#9902,0.225);
#3876=CIRCLE('',#9903,0.225);
#3877=CIRCLE('',#9905,0.225);
#3878=CIRCLE('',#9906,0.225);
#3879=CIRCLE('',#9908,1.59);
#3880=CIRCLE('',#9909,1.59);
#3881=CIRCLE('',#9911,1.005);
#3882=CIRCLE('',#9913,1.005);
#3883=CIRCLE('',#9915,2.4);
#3884=CIRCLE('',#9916,2.4);
#3885=CIRCLE('',#9921,0.225);
#3886=CIRCLE('',#9922,0.225);
#3887=CIRCLE('',#9924,0.225);
#3888=CIRCLE('',#9925,0.225);
#3889=CIRCLE('',#9927,0.225);
#3890=CIRCLE('',#9928,0.225);
#3891=CIRCLE('',#9930,0.225);
#3892=CIRCLE('',#9931,0.225);
#3893=CIRCLE('',#9933,1.59);
#3894=CIRCLE('',#9934,1.59);
#3895=CIRCLE('',#9936,1.005);
#3896=CIRCLE('',#9938,1.005);
#3897=CIRCLE('',#9940,2.4);
#3898=CIRCLE('',#9941,2.4);
#3899=CIRCLE('',#9946,0.6);
#3900=CIRCLE('',#9947,0.5);
#3901=CIRCLE('',#9949,0.6);
#3902=CIRCLE('',#9952,0.5);
#3903=CIRCLE('',#9957,1.070235);
#3904=CIRCLE('',#9958,1.070235);
#3905=CIRCLE('',#9959,0.309556);
#3906=CIRCLE('',#9960,1.070235);
#3907=CIRCLE('',#9961,1.070235);
#3908=CIRCLE('',#9963,1.070235);
#3909=CIRCLE('',#9965,0.6);
#3910=CIRCLE('',#9966,0.6);
#3911=CIRCLE('',#9968,0.66);
#3912=CIRCLE('',#9971,1.070235);
#3913=CIRCLE('',#9973,0.66);
#3914=CIRCLE('',#9977,1.129765);
#3915=CIRCLE('',#9978,1.129765);
#3916=CIRCLE('',#9979,0.309556);
#3917=CIRCLE('',#9980,1.129765);
#3918=CIRCLE('',#9981,1.129765);
#3919=CIRCLE('',#9983,1.129765);
#3920=CIRCLE('',#9985,1.54);
#3921=CIRCLE('',#9986,1.129765);
#3922=CIRCLE('',#9988,1.6);
#3923=CIRCLE('',#9990,1.6);
#3924=CIRCLE('',#9992,1.54);
#3925=CIRCLE('',#9997,0.29765);
#3926=CIRCLE('',#9999,0.29765);
#3927=CIRCLE('',#10001,0.29765);
#3928=CIRCLE('',#10003,0.29765);
#3929=CIRCLE('',#10005,0.29765);
#3930=CIRCLE('',#10007,0.29765);
#3931=CIRCLE('',#10009,0.29765);
#3932=CIRCLE('',#10012,0.303778037777585);
#3933=CIRCLE('',#10013,0.303778037777585);
#3934=CIRCLE('',#10015,1.123812);
#3935=CIRCLE('',#10016,1.123812);
#3936=CIRCLE('',#10017,1.123812);
#3937=CIRCLE('',#10018,1.123812);
#3938=CIRCLE('',#10019,1.123812);
#3939=CIRCLE('',#10020,1.123812);
#3940=CIRCLE('',#10021,1.123812);
#3941=CIRCLE('',#10022,1.123812);
#3942=CIRCLE('',#10023,1.123812);
#3943=CIRCLE('',#10025,1.076188);
#3944=CIRCLE('',#10026,0.303778037777585);
#3945=CIRCLE('',#10028,0.303778037777585);
#3946=CIRCLE('',#10030,1.076188);
#3947=CIRCLE('',#10031,0.303778037777585);
#3948=CIRCLE('',#10033,0.303778037777585);
#3949=CIRCLE('',#10035,1.076188);
#3950=CIRCLE('',#10036,1.076188);
#3951=CIRCLE('',#10037,0.303778037777585);
#3952=CIRCLE('',#10039,0.303778037777585);
#3953=CIRCLE('',#10041,1.076188);
#3954=CIRCLE('',#10042,0.303778037777585);
#3955=CIRCLE('',#10044,0.303778037777585);
#3956=CIRCLE('',#10046,1.076188);
#3957=CIRCLE('',#10047,0.303778037777585);
#3958=CIRCLE('',#10049,0.303778037777585);
#3959=CIRCLE('',#10051,1.076188);
#3960=CIRCLE('',#10052,1.076188);
#3961=CIRCLE('',#10053,1.076188);
#3962=CIRCLE('',#10055,0.303778037777585);
#3963=CIRCLE('',#10057,0.303778037777585);
#3964=CIRCLE('',#10062,1.119765);
#3965=CIRCLE('',#10063,1.085235);
#3966=CIRCLE('',#10065,1.119765);
#3967=CIRCLE('',#10067,1.085235);
#3968=CIRCLE('',#10070,1.119765);
#3969=CIRCLE('',#10071,1.085235);
#3970=CIRCLE('',#10073,1.119765);
#3971=CIRCLE('',#10075,1.085235);
#3972=CIRCLE('',#10085,0.165);
#3973=CIRCLE('',#10086,0.165);
#3974=CIRCLE('',#10089,0.164999999999999);
#3975=CIRCLE('',#10090,0.164999999999999);
#3976=CIRCLE('',#10093,0.165);
#3977=CIRCLE('',#10094,0.165);
#3978=CIRCLE('',#10097,0.164999999999999);
#3979=CIRCLE('',#10098,0.164999999999999);
#3980=CIRCLE('',#10101,0.165);
#3981=CIRCLE('',#10102,0.165);
#3982=CIRCLE('',#10105,0.165);
#3983=CIRCLE('',#10106,0.165);
#3984=CIRCLE('',#10109,0.165);
#3985=CIRCLE('',#10110,0.165);
#3986=CIRCLE('',#10112,0.165);
#3987=CIRCLE('',#10113,0.165);
#3988=CIRCLE('',#10115,0.165);
#3989=CIRCLE('',#10116,0.165);
#3990=CIRCLE('',#10118,0.165);
#3991=CIRCLE('',#10119,0.165);
#3992=CIRCLE('',#10121,1.1);
#3993=CIRCLE('',#10122,1.1);
#3994=CIRCLE('',#10124,1.05);
#3995=CIRCLE('',#10125,1.05);
#3996=CIRCLE('',#10127,1.05);
#3997=CIRCLE('',#10128,1.05);
#3998=CIRCLE('',#10137,0.225);
#3999=CIRCLE('',#10138,0.225);
#4000=CIRCLE('',#10140,0.225);
#4001=CIRCLE('',#10141,0.225);
#4002=CIRCLE('',#10143,0.225);
#4003=CIRCLE('',#10144,0.225);
#4004=CIRCLE('',#10146,0.225);
#4005=CIRCLE('',#10147,0.225);
#4006=CIRCLE('',#10149,1.65);
#4007=CIRCLE('',#10150,1.65);
#4008=CIRCLE('',#10152,0.7);
#4009=CIRCLE('',#10153,0.7);
#4010=CIRCLE('',#10155,0.7);
#4011=CIRCLE('',#10156,0.7);
#4012=CIRCLE('',#10165,0.225);
#4013=CIRCLE('',#10166,0.225);
#4014=CIRCLE('',#10168,0.225);
#4015=CIRCLE('',#10169,0.225);
#4016=CIRCLE('',#10171,0.225);
#4017=CIRCLE('',#10172,0.225);
#4018=CIRCLE('',#10174,0.225);
#4019=CIRCLE('',#10175,0.225);
#4020=CIRCLE('',#10177,1.65);
#4021=CIRCLE('',#10178,1.65);
#4022=CIRCLE('',#10180,0.7);
#4023=CIRCLE('',#10181,0.7);
#4024=CIRCLE('',#10183,0.7);
#4025=CIRCLE('',#10184,0.7);
#4026=CIRCLE('',#10193,1.1);
#4027=CIRCLE('',#10194,0.225);
#4028=CIRCLE('',#10195,0.225);
#4029=CIRCLE('',#10197,0.225);
#4030=CIRCLE('',#10198,0.225);
#4031=CIRCLE('',#10200,1.1);
#4032=CIRCLE('',#10201,0.225);
#4033=CIRCLE('',#10202,1.1);
#4034=CIRCLE('',#10204,0.225);
#4035=CIRCLE('',#10205,0.225);
#4036=CIRCLE('',#10206,0.225);
#4037=CIRCLE('',#10208,1.1);
#4038=CIRCLE('',#10209,1.1);
#4039=CIRCLE('',#10210,1.1);
#4040=CIRCLE('',#10212,1.6);
#4041=CIRCLE('',#10214,1.6);
#4042=CIRCLE('',#10216,0.525);
#4043=CIRCLE('',#10218,0.525);
#4044=CIRCLE('',#10222,0.4);
#4045=CIRCLE('',#10223,0.4);
#4046=CIRCLE('',#10225,0.225);
#4047=CIRCLE('',#10227,0.4);
#4048=CIRCLE('',#10228,0.4);
#4049=CIRCLE('',#10230,0.225);
#4050=CIRCLE('',#10232,0.4);
#4051=CIRCLE('',#10233,0.4);
#4052=CIRCLE('',#10235,0.225);
#4053=CIRCLE('',#10237,0.4);
#4054=CIRCLE('',#10238,0.4);
#4055=CIRCLE('',#10240,0.225);
#4056=CIRCLE('',#10242,0.225);
#4057=CIRCLE('',#10244,0.225);
#4058=CIRCLE('',#10246,0.225);
#4059=CIRCLE('',#10248,0.225);
#4060=CIRCLE('',#10258,0.165);
#4061=CIRCLE('',#10259,0.165);
#4062=CIRCLE('',#10262,0.164999999999999);
#4063=CIRCLE('',#10263,0.164999999999999);
#4064=CIRCLE('',#10266,0.165);
#4065=CIRCLE('',#10267,0.165);
#4066=CIRCLE('',#10270,0.164999999999999);
#4067=CIRCLE('',#10271,0.164999999999999);
#4068=CIRCLE('',#10274,0.165);
#4069=CIRCLE('',#10275,0.165);
#4070=CIRCLE('',#10278,0.165);
#4071=CIRCLE('',#10279,0.165);
#4072=CIRCLE('',#10282,0.165);
#4073=CIRCLE('',#10283,0.165);
#4074=CIRCLE('',#10285,0.165);
#4075=CIRCLE('',#10286,0.165);
#4076=CIRCLE('',#10288,0.165);
#4077=CIRCLE('',#10289,0.165);
#4078=CIRCLE('',#10291,0.165);
#4079=CIRCLE('',#10292,0.165);
#4080=CIRCLE('',#10294,1.1);
#4081=CIRCLE('',#10295,1.1);
#4082=CIRCLE('',#10297,1.05);
#4083=CIRCLE('',#10298,1.05);
#4084=CIRCLE('',#10300,1.05);
#4085=CIRCLE('',#10301,1.05);
#4086=CIRCLE('',#10310,0.225);
#4087=CIRCLE('',#10311,0.225);
#4088=CIRCLE('',#10313,0.225);
#4089=CIRCLE('',#10314,0.225);
#4090=CIRCLE('',#10316,0.225);
#4091=CIRCLE('',#10317,0.225);
#4092=CIRCLE('',#10319,0.225);
#4093=CIRCLE('',#10320,0.225);
#4094=CIRCLE('',#10322,1.65);
#4095=CIRCLE('',#10323,1.65);
#4096=CIRCLE('',#10325,0.7);
#4097=CIRCLE('',#10326,0.7);
#4098=CIRCLE('',#10328,0.7);
#4099=CIRCLE('',#10329,0.7);
#4100=CIRCLE('',#10338,0.225);
#4101=CIRCLE('',#10339,0.225);
#4102=CIRCLE('',#10341,0.225);
#4103=CIRCLE('',#10342,0.225);
#4104=CIRCLE('',#10344,0.225);
#4105=CIRCLE('',#10345,0.225);
#4106=CIRCLE('',#10347,0.225);
#4107=CIRCLE('',#10348,0.225);
#4108=CIRCLE('',#10350,1.65);
#4109=CIRCLE('',#10351,1.65);
#4110=CIRCLE('',#10353,0.7);
#4111=CIRCLE('',#10354,0.7);
#4112=CIRCLE('',#10356,0.7);
#4113=CIRCLE('',#10357,0.7);
#4114=CIRCLE('',#10366,1.1);
#4115=CIRCLE('',#10367,0.225);
#4116=CIRCLE('',#10368,0.225);
#4117=CIRCLE('',#10370,0.225);
#4118=CIRCLE('',#10371,0.225);
#4119=CIRCLE('',#10373,1.1);
#4120=CIRCLE('',#10374,0.225);
#4121=CIRCLE('',#10375,1.1);
#4122=CIRCLE('',#10377,0.225);
#4123=CIRCLE('',#10378,0.225);
#4124=CIRCLE('',#10379,0.225);
#4125=CIRCLE('',#10381,1.1);
#4126=CIRCLE('',#10382,1.1);
#4127=CIRCLE('',#10383,1.1);
#4128=CIRCLE('',#10385,1.6);
#4129=CIRCLE('',#10387,1.6);
#4130=CIRCLE('',#10389,0.525);
#4131=CIRCLE('',#10391,0.525);
#4132=CIRCLE('',#10395,0.4);
#4133=CIRCLE('',#10396,0.4);
#4134=CIRCLE('',#10398,0.225);
#4135=CIRCLE('',#10400,0.4);
#4136=CIRCLE('',#10401,0.4);
#4137=CIRCLE('',#10403,0.225);
#4138=CIRCLE('',#10405,0.4);
#4139=CIRCLE('',#10406,0.4);
#4140=CIRCLE('',#10408,0.225);
#4141=CIRCLE('',#10410,0.4);
#4142=CIRCLE('',#10411,0.4);
#4143=CIRCLE('',#10413,0.225);
#4144=CIRCLE('',#10415,0.225);
#4145=CIRCLE('',#10417,0.225);
#4146=CIRCLE('',#10419,0.225);
#4147=CIRCLE('',#10421,0.225);
#4148=CIRCLE('',#10431,0.9);
#4149=CIRCLE('',#10434,0.9);
#4150=CIRCLE('',#10438,1.05);
#4151=CIRCLE('',#10439,0.9);
#4152=CIRCLE('',#10441,1.05);
#4153=CIRCLE('',#10443,1.);
#4154=CIRCLE('',#10445,1.);
#4155=CIRCLE('',#10447,1.05);
#4156=CIRCLE('',#10449,1.05);
#4157=CIRCLE('',#10451,1.);
#4158=CIRCLE('',#10453,1.);
#4159=CIRCLE('',#10455,1.05);
#4160=CIRCLE('',#10457,1.05);
#4161=CIRCLE('',#10459,0.9);
#4162=CIRCLE('',#10463,0.895);
#4163=CIRCLE('',#10464,0.605);
#4164=CIRCLE('',#10467,0.895);
#4165=CIRCLE('',#10468,0.605);
#4166=CIRCLE('',#10471,0.895);
#4167=CIRCLE('',#10472,0.605);
#4168=CIRCLE('',#10474,0.895);
#4169=CIRCLE('',#10476,0.605);
#4170=CIRCLE('',#10490,0.1954);
#4171=CIRCLE('',#10492,0.3);
#4172=CIRCLE('',#10494,0.35);
#4173=CIRCLE('',#10496,0.35);
#4174=CIRCLE('',#10498,0.32);
#4175=CIRCLE('',#10500,0.22);
#4176=CIRCLE('',#10502,0.1954);
#4177=CIRCLE('',#10507,0.165);
#4178=CIRCLE('',#10508,0.165);
#4179=CIRCLE('',#10511,0.165);
#4180=CIRCLE('',#10512,0.165);
#4181=CIRCLE('',#10515,0.8);
#4182=CIRCLE('',#10516,0.6);
#4183=CIRCLE('',#10518,0.8);
#4184=CIRCLE('',#10519,0.6);
#4185=CIRCLE('',#10522,0.6);
#4186=CIRCLE('',#10524,0.8);
#4187=CIRCLE('',#10526,0.8);
#4188=CIRCLE('',#10527,0.6);
#4189=CIRCLE('',#10530,0.6);
#4190=CIRCLE('',#10532,0.6);
#4191=CIRCLE('',#10537,0.605);
#4192=CIRCLE('',#10538,0.605);
#4193=CIRCLE('',#10540,0.8);
#4194=CIRCLE('',#10541,0.8);
#4195=CIRCLE('',#10546,0.605);
#4196=CIRCLE('',#10547,0.605);
#4197=CIRCLE('',#10549,0.8);
#4198=CIRCLE('',#10550,0.8);
#4199=CIRCLE('',#10555,2.3);
#4200=CIRCLE('',#10556,2.3);
#4201=CIRCLE('',#10558,0.164999999999999);
#4202=CIRCLE('',#10560,0.164999999999999);
#4203=CIRCLE('',#10563,1.2);
#4204=CIRCLE('',#10565,0.6);
#4205=CIRCLE('',#10566,0.6);
#4206=CIRCLE('',#10568,1.2);
#4207=CIRCLE('',#10573,0.225);
#4208=CIRCLE('',#10574,0.225);
#4209=CIRCLE('',#10576,1.);
#4210=CIRCLE('',#10577,1.);
#4211=CIRCLE('',#10582,0.225);
#4212=CIRCLE('',#10583,0.225);
#4213=CIRCLE('',#10585,1.);
#4214=CIRCLE('',#10586,1.);
#4215=CIRCLE('',#10591,0.164999999999999);
#4216=CIRCLE('',#10593,0.164999999999999);
#4217=CIRCLE('',#10596,0.605);
#4218=CIRCLE('',#10597,0.605);
#4219=CIRCLE('',#10599,1.);
#4220=CIRCLE('',#10600,1.);
#4221=CIRCLE('',#10605,0.3);
#4222=CIRCLE('',#10607,0.35);
#4223=CIRCLE('',#10609,0.35);
#4224=CIRCLE('',#10611,0.32);
#4225=CIRCLE('',#10613,0.22);
#4226=CIRCLE('',#10615,0.1954);
#4227=CIRCLE('',#10617,0.1954);
#4228=CIRCLE('',#10619,0.16);
#4229=CIRCLE('',#10680,0.17);
#4230=CIRCLE('',#10682,0.1954);
#4231=CIRCLE('',#10684,0.1954);
#4232=CIRCLE('',#10686,0.125);
#4233=VERTEX_POINT('',#13679);
#4234=VERTEX_POINT('',#13681);
#4235=VERTEX_POINT('',#13685);
#4236=VERTEX_POINT('',#13687);
#4237=VERTEX_POINT('',#13691);
#4238=VERTEX_POINT('',#13693);
#4239=VERTEX_POINT('',#13697);
#4240=VERTEX_POINT('',#13699);
#4241=VERTEX_POINT('',#13703);
#4242=VERTEX_POINT('',#13705);
#4243=VERTEX_POINT('',#13709);
#4244=VERTEX_POINT('',#13711);
#4245=VERTEX_POINT('',#13715);
#4246=VERTEX_POINT('',#13717);
#4247=VERTEX_POINT('',#13721);
#4248=VERTEX_POINT('',#13723);
#4249=VERTEX_POINT('',#13727);
#4250=VERTEX_POINT('',#13729);
#4251=VERTEX_POINT('',#13733);
#4252=VERTEX_POINT('',#13735);
#4253=VERTEX_POINT('',#13739);
#4254=VERTEX_POINT('',#13741);
#4255=VERTEX_POINT('',#13745);
#4256=VERTEX_POINT('',#13747);
#4257=VERTEX_POINT('',#13751);
#4258=VERTEX_POINT('',#13752);
#4259=VERTEX_POINT('',#13754);
#4260=VERTEX_POINT('',#13756);
#4261=VERTEX_POINT('',#13760);
#4262=VERTEX_POINT('',#13762);
#4263=VERTEX_POINT('',#13766);
#4264=VERTEX_POINT('',#13768);
#4265=VERTEX_POINT('',#13778);
#4266=VERTEX_POINT('',#13779);
#4267=VERTEX_POINT('',#13781);
#4268=VERTEX_POINT('',#13783);
#4269=VERTEX_POINT('',#13787);
#4270=VERTEX_POINT('',#13789);
#4271=VERTEX_POINT('',#13793);
#4272=VERTEX_POINT('',#13795);
#4273=VERTEX_POINT('',#13805);
#4274=VERTEX_POINT('',#13806);
#4275=VERTEX_POINT('',#13808);
#4276=VERTEX_POINT('',#13810);
#4277=VERTEX_POINT('',#13814);
#4278=VERTEX_POINT('',#13816);
#4279=VERTEX_POINT('',#13820);
#4280=VERTEX_POINT('',#13822);
#4281=VERTEX_POINT('',#13832);
#4282=VERTEX_POINT('',#13833);
#4283=VERTEX_POINT('',#13835);
#4284=VERTEX_POINT('',#13837);
#4285=VERTEX_POINT('',#13841);
#4286=VERTEX_POINT('',#13842);
#4287=VERTEX_POINT('',#13844);
#4288=VERTEX_POINT('',#13846);
#4289=VERTEX_POINT('',#13850);
#4290=VERTEX_POINT('',#13851);
#4291=VERTEX_POINT('',#13855);
#4292=VERTEX_POINT('',#13856);
#4293=VERTEX_POINT('',#13863);
#4294=VERTEX_POINT('',#13865);
#4295=VERTEX_POINT('',#13884);
#4296=VERTEX_POINT('',#13894);
#4297=VERTEX_POINT('',#13901);
#4298=VERTEX_POINT('',#13904);
#4299=VERTEX_POINT('',#13905);
#4300=VERTEX_POINT('',#13908);
#4301=VERTEX_POINT('',#13910);
#4302=VERTEX_POINT('',#13915);
#4303=VERTEX_POINT('',#13919);
#4304=VERTEX_POINT('',#13923);
#4305=VERTEX_POINT('',#13926);
#4306=VERTEX_POINT('',#13930);
#4307=VERTEX_POINT('',#13931);
#4308=VERTEX_POINT('',#13936);
#4309=VERTEX_POINT('',#13940);
#4310=VERTEX_POINT('',#13948);
#4311=VERTEX_POINT('',#13949);
#4312=VERTEX_POINT('',#13951);
#4313=VERTEX_POINT('',#13953);
#4314=VERTEX_POINT('',#13957);
#4315=VERTEX_POINT('',#13958);
#4316=VERTEX_POINT('',#13960);
#4317=VERTEX_POINT('',#13962);
#4318=VERTEX_POINT('',#13966);
#4319=VERTEX_POINT('',#13967);
#4320=VERTEX_POINT('',#13971);
#4321=VERTEX_POINT('',#13972);
#4322=VERTEX_POINT('',#13979);
#4323=VERTEX_POINT('',#13981);
#4324=VERTEX_POINT('',#14000);
#4325=VERTEX_POINT('',#14010);
#4326=VERTEX_POINT('',#14017);
#4327=VERTEX_POINT('',#14020);
#4328=VERTEX_POINT('',#14021);
#4329=VERTEX_POINT('',#14024);
#4330=VERTEX_POINT('',#14026);
#4331=VERTEX_POINT('',#14031);
#4332=VERTEX_POINT('',#14035);
#4333=VERTEX_POINT('',#14039);
#4334=VERTEX_POINT('',#14042);
#4335=VERTEX_POINT('',#14046);
#4336=VERTEX_POINT('',#14047);
#4337=VERTEX_POINT('',#14052);
#4338=VERTEX_POINT('',#14056);
#4339=VERTEX_POINT('',#14064);
#4340=VERTEX_POINT('',#14065);
#4341=VERTEX_POINT('',#14067);
#4342=VERTEX_POINT('',#14069);
#4343=VERTEX_POINT('',#14073);
#4344=VERTEX_POINT('',#14074);
#4345=VERTEX_POINT('',#14076);
#4346=VERTEX_POINT('',#14078);
#4347=VERTEX_POINT('',#14082);
#4348=VERTEX_POINT('',#14083);
#4349=VERTEX_POINT('',#14087);
#4350=VERTEX_POINT('',#14088);
#4351=VERTEX_POINT('',#14095);
#4352=VERTEX_POINT('',#14097);
#4353=VERTEX_POINT('',#14116);
#4354=VERTEX_POINT('',#14126);
#4355=VERTEX_POINT('',#14133);
#4356=VERTEX_POINT('',#14136);
#4357=VERTEX_POINT('',#14137);
#4358=VERTEX_POINT('',#14140);
#4359=VERTEX_POINT('',#14142);
#4360=VERTEX_POINT('',#14147);
#4361=VERTEX_POINT('',#14151);
#4362=VERTEX_POINT('',#14155);
#4363=VERTEX_POINT('',#14158);
#4364=VERTEX_POINT('',#14162);
#4365=VERTEX_POINT('',#14163);
#4366=VERTEX_POINT('',#14168);
#4367=VERTEX_POINT('',#14172);
#4368=VERTEX_POINT('',#14180);
#4369=VERTEX_POINT('',#14181);
#4370=VERTEX_POINT('',#14183);
#4371=VERTEX_POINT('',#14185);
#4372=VERTEX_POINT('',#14189);
#4373=VERTEX_POINT('',#14190);
#4374=VERTEX_POINT('',#14192);
#4375=VERTEX_POINT('',#14194);
#4376=VERTEX_POINT('',#14198);
#4377=VERTEX_POINT('',#14199);
#4378=VERTEX_POINT('',#14203);
#4379=VERTEX_POINT('',#14204);
#4380=VERTEX_POINT('',#14211);
#4381=VERTEX_POINT('',#14213);
#4382=VERTEX_POINT('',#14232);
#4383=VERTEX_POINT('',#14242);
#4384=VERTEX_POINT('',#14249);
#4385=VERTEX_POINT('',#14252);
#4386=VERTEX_POINT('',#14253);
#4387=VERTEX_POINT('',#14256);
#4388=VERTEX_POINT('',#14258);
#4389=VERTEX_POINT('',#14263);
#4390=VERTEX_POINT('',#14267);
#4391=VERTEX_POINT('',#14271);
#4392=VERTEX_POINT('',#14274);
#4393=VERTEX_POINT('',#14278);
#4394=VERTEX_POINT('',#14279);
#4395=VERTEX_POINT('',#14284);
#4396=VERTEX_POINT('',#14288);
#4397=VERTEX_POINT('',#14296);
#4398=VERTEX_POINT('',#14298);
#4399=VERTEX_POINT('',#14302);
#4400=VERTEX_POINT('',#14304);
#4401=VERTEX_POINT('',#14308);
#4402=VERTEX_POINT('',#14310);
#4403=VERTEX_POINT('',#14314);
#4404=VERTEX_POINT('',#14316);
#4405=VERTEX_POINT('',#14320);
#4406=VERTEX_POINT('',#14322);
#4407=VERTEX_POINT('',#14326);
#4408=VERTEX_POINT('',#14328);
#4409=VERTEX_POINT('',#14332);
#4410=VERTEX_POINT('',#14334);
#4411=VERTEX_POINT('',#14338);
#4412=VERTEX_POINT('',#14339);
#4413=VERTEX_POINT('',#14341);
#4414=VERTEX_POINT('',#14343);
#4415=VERTEX_POINT('',#14347);
#4416=VERTEX_POINT('',#14348);
#4417=VERTEX_POINT('',#14350);
#4418=VERTEX_POINT('',#14352);
#4419=VERTEX_POINT('',#14356);
#4420=VERTEX_POINT('',#14358);
#4421=VERTEX_POINT('',#14362);
#4422=VERTEX_POINT('',#14364);
#4423=VERTEX_POINT('',#14368);
#4424=VERTEX_POINT('',#14370);
#4425=VERTEX_POINT('',#14374);
#4426=VERTEX_POINT('',#14379);
#4427=VERTEX_POINT('',#14389);
#4428=VERTEX_POINT('',#14391);
#4429=VERTEX_POINT('',#14395);
#4430=VERTEX_POINT('',#14397);
#4431=VERTEX_POINT('',#14401);
#4432=VERTEX_POINT('',#14403);
#4433=VERTEX_POINT('',#14407);
#4434=VERTEX_POINT('',#14409);
#4435=VERTEX_POINT('',#14413);
#4436=VERTEX_POINT('',#14415);
#4437=VERTEX_POINT('',#14419);
#4438=VERTEX_POINT('',#14422);
#4439=VERTEX_POINT('',#14426);
#4440=VERTEX_POINT('',#14428);
#4441=VERTEX_POINT('',#14435);
#4442=VERTEX_POINT('',#14437);
#4443=VERTEX_POINT('',#14441);
#4444=VERTEX_POINT('',#14443);
#4445=VERTEX_POINT('',#14447);
#4446=VERTEX_POINT('',#14449);
#4447=VERTEX_POINT('',#14453);
#4448=VERTEX_POINT('',#14455);
#4449=VERTEX_POINT('',#14459);
#4450=VERTEX_POINT('',#14461);
#4451=VERTEX_POINT('',#14465);
#4452=VERTEX_POINT('',#14468);
#4453=VERTEX_POINT('',#14472);
#4454=VERTEX_POINT('',#14474);
#4455=VERTEX_POINT('',#14481);
#4456=VERTEX_POINT('',#14483);
#4457=VERTEX_POINT('',#14487);
#4458=VERTEX_POINT('',#14489);
#4459=VERTEX_POINT('',#14493);
#4460=VERTEX_POINT('',#14495);
#4461=VERTEX_POINT('',#14499);
#4462=VERTEX_POINT('',#14501);
#4463=VERTEX_POINT('',#14505);
#4464=VERTEX_POINT('',#14507);
#4465=VERTEX_POINT('',#14511);
#4466=VERTEX_POINT('',#14513);
#4467=VERTEX_POINT('',#14517);
#4468=VERTEX_POINT('',#14519);
#4469=VERTEX_POINT('',#14523);
#4470=VERTEX_POINT('',#14524);
#4471=VERTEX_POINT('',#14526);
#4472=VERTEX_POINT('',#14528);
#4473=VERTEX_POINT('',#14532);
#4474=VERTEX_POINT('',#14533);
#4475=VERTEX_POINT('',#14535);
#4476=VERTEX_POINT('',#14537);
#4477=VERTEX_POINT('',#14541);
#4478=VERTEX_POINT('',#14543);
#4479=VERTEX_POINT('',#14547);
#4480=VERTEX_POINT('',#14549);
#4481=VERTEX_POINT('',#14553);
#4482=VERTEX_POINT('',#14555);
#4483=VERTEX_POINT('',#14559);
#4484=VERTEX_POINT('',#14564);
#4485=VERTEX_POINT('',#14574);
#4486=VERTEX_POINT('',#14576);
#4487=VERTEX_POINT('',#14580);
#4488=VERTEX_POINT('',#14582);
#4489=VERTEX_POINT('',#14586);
#4490=VERTEX_POINT('',#14588);
#4491=VERTEX_POINT('',#14592);
#4492=VERTEX_POINT('',#14594);
#4493=VERTEX_POINT('',#14598);
#4494=VERTEX_POINT('',#14600);
#4495=VERTEX_POINT('',#14604);
#4496=VERTEX_POINT('',#14607);
#4497=VERTEX_POINT('',#14611);
#4498=VERTEX_POINT('',#14613);
#4499=VERTEX_POINT('',#14620);
#4500=VERTEX_POINT('',#14622);
#4501=VERTEX_POINT('',#14626);
#4502=VERTEX_POINT('',#14628);
#4503=VERTEX_POINT('',#14632);
#4504=VERTEX_POINT('',#14634);
#4505=VERTEX_POINT('',#14638);
#4506=VERTEX_POINT('',#14640);
#4507=VERTEX_POINT('',#14644);
#4508=VERTEX_POINT('',#14646);
#4509=VERTEX_POINT('',#14650);
#4510=VERTEX_POINT('',#14653);
#4511=VERTEX_POINT('',#14657);
#4512=VERTEX_POINT('',#14659);
#4513=VERTEX_POINT('',#14666);
#4514=VERTEX_POINT('',#14668);
#4515=VERTEX_POINT('',#14672);
#4516=VERTEX_POINT('',#14677);
#4517=VERTEX_POINT('',#14684);
#4518=VERTEX_POINT('',#14685);
#4519=VERTEX_POINT('',#14688);
#4520=VERTEX_POINT('',#14690);
#4521=VERTEX_POINT('',#14694);
#4522=VERTEX_POINT('',#14698);
#4523=VERTEX_POINT('',#14700);
#4524=VERTEX_POINT('',#14704);
#4525=VERTEX_POINT('',#14709);
#4526=VERTEX_POINT('',#14713);
#4527=VERTEX_POINT('',#14719);
#4528=VERTEX_POINT('',#14720);
#4529=VERTEX_POINT('',#14723);
#4530=VERTEX_POINT('',#14725);
#4531=VERTEX_POINT('',#14729);
#4532=VERTEX_POINT('',#14733);
#4533=VERTEX_POINT('',#14735);
#4534=VERTEX_POINT('',#14738);
#4535=VERTEX_POINT('',#14742);
#4536=VERTEX_POINT('',#14746);
#4537=VERTEX_POINT('',#14754);
#4538=VERTEX_POINT('',#14755);
#4539=VERTEX_POINT('',#14758);
#4540=VERTEX_POINT('',#14759);
#4541=VERTEX_POINT('',#14762);
#4542=VERTEX_POINT('',#14763);
#4543=VERTEX_POINT('',#14766);
#4544=VERTEX_POINT('',#14767);
#4545=VERTEX_POINT('',#14770);
#4546=VERTEX_POINT('',#14771);
#4547=VERTEX_POINT('',#14774);
#4548=VERTEX_POINT('',#14775);
#4549=VERTEX_POINT('',#14778);
#4550=VERTEX_POINT('',#14779);
#4551=VERTEX_POINT('',#14783);
#4552=VERTEX_POINT('',#14784);
#4553=VERTEX_POINT('',#14807);
#4554=VERTEX_POINT('',#14809);
#4555=VERTEX_POINT('',#14834);
#4556=VERTEX_POINT('',#14836);
#4557=VERTEX_POINT('',#14859);
#4558=VERTEX_POINT('',#14861);
#4559=VERTEX_POINT('',#14884);
#4560=VERTEX_POINT('',#14886);
#4561=VERTEX_POINT('',#14889);
#4562=VERTEX_POINT('',#14891);
#4563=VERTEX_POINT('',#14914);
#4564=VERTEX_POINT('',#14916);
#4565=VERTEX_POINT('',#14939);
#4566=VERTEX_POINT('',#14941);
#4567=VERTEX_POINT('',#14964);
#4568=VERTEX_POINT('',#14966);
#4569=VERTEX_POINT('',#14991);
#4570=VERTEX_POINT('',#14995);
#4571=VERTEX_POINT('',#15020);
#4572=VERTEX_POINT('',#15024);
#4573=VERTEX_POINT('',#15049);
#4574=VERTEX_POINT('',#15051);
#4575=VERTEX_POINT('',#15055);
#4576=VERTEX_POINT('',#15080);
#4577=VERTEX_POINT('',#15084);
#4578=VERTEX_POINT('',#15109);
#4579=VERTEX_POINT('',#15113);
#4580=VERTEX_POINT('',#15138);
#4581=VERTEX_POINT('',#15141);
#4582=VERTEX_POINT('',#15143);
#4583=VERTEX_POINT('',#15175);
#4584=VERTEX_POINT('',#15177);
#4585=VERTEX_POINT('',#15180);
#4586=VERTEX_POINT('',#15184);
#4587=VERTEX_POINT('',#15189);
#4588=VERTEX_POINT('',#15191);
#4589=VERTEX_POINT('',#15194);
#4590=VERTEX_POINT('',#15198);
#4591=VERTEX_POINT('',#15210);
#4592=VERTEX_POINT('',#15212);
#4593=VERTEX_POINT('',#15217);
#4594=VERTEX_POINT('',#15219);
#4595=VERTEX_POINT('',#15224);
#4596=VERTEX_POINT('',#15226);
#4597=VERTEX_POINT('',#15231);
#4598=VERTEX_POINT('',#15233);
#4599=VERTEX_POINT('',#15238);
#4600=VERTEX_POINT('',#15240);
#4601=VERTEX_POINT('',#15245);
#4602=VERTEX_POINT('',#15247);
#4603=VERTEX_POINT('',#15252);
#4604=VERTEX_POINT('',#15254);
#4605=VERTEX_POINT('',#15258);
#4606=VERTEX_POINT('',#15260);
#4607=VERTEX_POINT('',#15264);
#4608=VERTEX_POINT('',#15266);
#4609=VERTEX_POINT('',#15270);
#4610=VERTEX_POINT('',#15272);
#4611=VERTEX_POINT('',#15276);
#4612=VERTEX_POINT('',#15278);
#4613=VERTEX_POINT('',#15282);
#4614=VERTEX_POINT('',#15284);
#4615=VERTEX_POINT('',#15288);
#4616=VERTEX_POINT('',#15290);
#4617=VERTEX_POINT('',#15294);
#4618=VERTEX_POINT('',#15295);
#4619=VERTEX_POINT('',#15297);
#4620=VERTEX_POINT('',#15299);
#4621=VERTEX_POINT('',#15303);
#4622=VERTEX_POINT('',#15305);
#4623=VERTEX_POINT('',#15309);
#4624=VERTEX_POINT('',#15311);
#4625=VERTEX_POINT('',#15321);
#4626=VERTEX_POINT('',#15323);
#4627=VERTEX_POINT('',#15327);
#4628=VERTEX_POINT('',#15329);
#4629=VERTEX_POINT('',#15333);
#4630=VERTEX_POINT('',#15335);
#4631=VERTEX_POINT('',#15339);
#4632=VERTEX_POINT('',#15341);
#4633=VERTEX_POINT('',#15345);
#4634=VERTEX_POINT('',#15347);
#4635=VERTEX_POINT('',#15351);
#4636=VERTEX_POINT('',#15353);
#4637=VERTEX_POINT('',#15357);
#4638=VERTEX_POINT('',#15359);
#4639=VERTEX_POINT('',#15363);
#4640=VERTEX_POINT('',#15364);
#4641=VERTEX_POINT('',#15366);
#4642=VERTEX_POINT('',#15368);
#4643=VERTEX_POINT('',#15372);
#4644=VERTEX_POINT('',#15374);
#4645=VERTEX_POINT('',#15378);
#4646=VERTEX_POINT('',#15380);
#4647=VERTEX_POINT('',#15390);
#4648=VERTEX_POINT('',#15392);
#4649=VERTEX_POINT('',#15396);
#4650=VERTEX_POINT('',#15398);
#4651=VERTEX_POINT('',#15402);
#4652=VERTEX_POINT('',#15404);
#4653=VERTEX_POINT('',#15408);
#4654=VERTEX_POINT('',#15410);
#4655=VERTEX_POINT('',#15414);
#4656=VERTEX_POINT('',#15416);
#4657=VERTEX_POINT('',#15420);
#4658=VERTEX_POINT('',#15422);
#4659=VERTEX_POINT('',#15426);
#4660=VERTEX_POINT('',#15428);
#4661=VERTEX_POINT('',#15432);
#4662=VERTEX_POINT('',#15433);
#4663=VERTEX_POINT('',#15435);
#4664=VERTEX_POINT('',#15437);
#4665=VERTEX_POINT('',#15441);
#4666=VERTEX_POINT('',#15443);
#4667=VERTEX_POINT('',#15447);
#4668=VERTEX_POINT('',#15449);
#4669=VERTEX_POINT('',#15459);
#4670=VERTEX_POINT('',#15460);
#4671=VERTEX_POINT('',#15462);
#4672=VERTEX_POINT('',#15466);
#4673=VERTEX_POINT('',#15468);
#4674=VERTEX_POINT('',#15471);
#4675=VERTEX_POINT('',#15475);
#4676=VERTEX_POINT('',#15476);
#4677=VERTEX_POINT('',#15478);
#4678=VERTEX_POINT('',#15482);
#4679=VERTEX_POINT('',#15484);
#4680=VERTEX_POINT('',#15486);
#4681=VERTEX_POINT('',#15489);
#4682=VERTEX_POINT('',#15494);
#4683=VERTEX_POINT('',#15499);
#4684=VERTEX_POINT('',#15502);
#4685=VERTEX_POINT('',#15506);
#4686=VERTEX_POINT('',#15509);
#4687=VERTEX_POINT('',#15515);
#4688=VERTEX_POINT('',#15517);
#4689=VERTEX_POINT('',#15521);
#4690=VERTEX_POINT('',#15524);
#4691=VERTEX_POINT('',#15526);
#4692=VERTEX_POINT('',#15530);
#4693=VERTEX_POINT('',#15533);
#4694=VERTEX_POINT('',#15535);
#4695=VERTEX_POINT('',#15539);
#4696=VERTEX_POINT('',#15542);
#4697=VERTEX_POINT('',#15544);
#4698=VERTEX_POINT('',#15548);
#4699=VERTEX_POINT('',#15551);
#4700=VERTEX_POINT('',#15555);
#4701=VERTEX_POINT('',#15559);
#4702=VERTEX_POINT('',#15563);
#4703=VERTEX_POINT('',#15567);
#4704=VERTEX_POINT('',#15568);
#4705=VERTEX_POINT('',#15570);
#4706=VERTEX_POINT('',#15572);
#4707=VERTEX_POINT('',#15576);
#4708=VERTEX_POINT('',#15578);
#4709=VERTEX_POINT('',#15582);
#4710=VERTEX_POINT('',#15584);
#4711=VERTEX_POINT('',#15595);
#4712=VERTEX_POINT('',#15597);
#4713=VERTEX_POINT('',#15602);
#4714=VERTEX_POINT('',#15604);
#4715=VERTEX_POINT('',#15609);
#4716=VERTEX_POINT('',#15611);
#4717=VERTEX_POINT('',#15616);
#4718=VERTEX_POINT('',#15618);
#4719=VERTEX_POINT('',#15623);
#4720=VERTEX_POINT('',#15625);
#4721=VERTEX_POINT('',#15630);
#4722=VERTEX_POINT('',#15632);
#4723=VERTEX_POINT('',#15637);
#4724=VERTEX_POINT('',#15639);
#4725=VERTEX_POINT('',#15643);
#4726=VERTEX_POINT('',#15645);
#4727=VERTEX_POINT('',#15649);
#4728=VERTEX_POINT('',#15651);
#4729=VERTEX_POINT('',#15655);
#4730=VERTEX_POINT('',#15657);
#4731=VERTEX_POINT('',#15661);
#4732=VERTEX_POINT('',#15663);
#4733=VERTEX_POINT('',#15667);
#4734=VERTEX_POINT('',#15669);
#4735=VERTEX_POINT('',#15673);
#4736=VERTEX_POINT('',#15675);
#4737=VERTEX_POINT('',#15679);
#4738=VERTEX_POINT('',#15680);
#4739=VERTEX_POINT('',#15682);
#4740=VERTEX_POINT('',#15684);
#4741=VERTEX_POINT('',#15688);
#4742=VERTEX_POINT('',#15690);
#4743=VERTEX_POINT('',#15694);
#4744=VERTEX_POINT('',#15696);
#4745=VERTEX_POINT('',#15706);
#4746=VERTEX_POINT('',#15708);
#4747=VERTEX_POINT('',#15712);
#4748=VERTEX_POINT('',#15714);
#4749=VERTEX_POINT('',#15718);
#4750=VERTEX_POINT('',#15720);
#4751=VERTEX_POINT('',#15724);
#4752=VERTEX_POINT('',#15726);
#4753=VERTEX_POINT('',#15730);
#4754=VERTEX_POINT('',#15732);
#4755=VERTEX_POINT('',#15736);
#4756=VERTEX_POINT('',#15738);
#4757=VERTEX_POINT('',#15742);
#4758=VERTEX_POINT('',#15744);
#4759=VERTEX_POINT('',#15748);
#4760=VERTEX_POINT('',#15749);
#4761=VERTEX_POINT('',#15751);
#4762=VERTEX_POINT('',#15753);
#4763=VERTEX_POINT('',#15757);
#4764=VERTEX_POINT('',#15759);
#4765=VERTEX_POINT('',#15763);
#4766=VERTEX_POINT('',#15765);
#4767=VERTEX_POINT('',#15775);
#4768=VERTEX_POINT('',#15777);
#4769=VERTEX_POINT('',#15781);
#4770=VERTEX_POINT('',#15783);
#4771=VERTEX_POINT('',#15787);
#4772=VERTEX_POINT('',#15789);
#4773=VERTEX_POINT('',#15793);
#4774=VERTEX_POINT('',#15795);
#4775=VERTEX_POINT('',#15799);
#4776=VERTEX_POINT('',#15801);
#4777=VERTEX_POINT('',#15805);
#4778=VERTEX_POINT('',#15807);
#4779=VERTEX_POINT('',#15811);
#4780=VERTEX_POINT('',#15813);
#4781=VERTEX_POINT('',#15817);
#4782=VERTEX_POINT('',#15818);
#4783=VERTEX_POINT('',#15820);
#4784=VERTEX_POINT('',#15822);
#4785=VERTEX_POINT('',#15826);
#4786=VERTEX_POINT('',#15828);
#4787=VERTEX_POINT('',#15832);
#4788=VERTEX_POINT('',#15834);
#4789=VERTEX_POINT('',#15844);
#4790=VERTEX_POINT('',#15845);
#4791=VERTEX_POINT('',#15847);
#4792=VERTEX_POINT('',#15851);
#4793=VERTEX_POINT('',#15854);
#4794=VERTEX_POINT('',#15856);
#4795=VERTEX_POINT('',#15860);
#4796=VERTEX_POINT('',#15861);
#4797=VERTEX_POINT('',#15863);
#4798=VERTEX_POINT('',#15867);
#4799=VERTEX_POINT('',#15869);
#4800=VERTEX_POINT('',#15871);
#4801=VERTEX_POINT('',#15874);
#4802=VERTEX_POINT('',#15878);
#4803=VERTEX_POINT('',#15884);
#4804=VERTEX_POINT('',#15887);
#4805=VERTEX_POINT('',#15891);
#4806=VERTEX_POINT('',#15894);
#4807=VERTEX_POINT('',#15900);
#4808=VERTEX_POINT('',#15902);
#4809=VERTEX_POINT('',#15906);
#4810=VERTEX_POINT('',#15909);
#4811=VERTEX_POINT('',#15911);
#4812=VERTEX_POINT('',#15915);
#4813=VERTEX_POINT('',#15918);
#4814=VERTEX_POINT('',#15920);
#4815=VERTEX_POINT('',#15924);
#4816=VERTEX_POINT('',#15927);
#4817=VERTEX_POINT('',#15929);
#4818=VERTEX_POINT('',#15933);
#4819=VERTEX_POINT('',#15936);
#4820=VERTEX_POINT('',#15940);
#4821=VERTEX_POINT('',#15944);
#4822=VERTEX_POINT('',#15948);
#4823=VERTEX_POINT('',#15952);
#4824=VERTEX_POINT('',#15953);
#4825=VERTEX_POINT('',#15955);
#4826=VERTEX_POINT('',#15957);
#4827=VERTEX_POINT('',#15961);
#4828=VERTEX_POINT('',#15963);
#4829=VERTEX_POINT('',#15967);
#4830=VERTEX_POINT('',#15969);
#4831=VERTEX_POINT('',#15980);
#4832=VERTEX_POINT('',#15981);
#4833=VERTEX_POINT('',#15983);
#4834=VERTEX_POINT('',#15985);
#4835=VERTEX_POINT('',#15989);
#4836=VERTEX_POINT('',#15991);
#4837=VERTEX_POINT('',#15995);
#4838=VERTEX_POINT('',#15997);
#4839=VERTEX_POINT('',#16005);
#4840=VERTEX_POINT('',#16007);
#4841=VERTEX_POINT('',#16010);
#4842=VERTEX_POINT('',#16014);
#4843=VERTEX_POINT('',#16017);
#4844=VERTEX_POINT('',#16021);
#4845=VERTEX_POINT('',#16024);
#4846=VERTEX_POINT('',#16028);
#4847=VERTEX_POINT('',#16031);
#4848=VERTEX_POINT('',#16035);
#4849=VERTEX_POINT('',#16038);
#4850=VERTEX_POINT('',#16042);
#4851=VERTEX_POINT('',#16048);
#4852=VERTEX_POINT('',#16049);
#4853=VERTEX_POINT('',#16051);
#4854=VERTEX_POINT('',#16053);
#4855=VERTEX_POINT('',#16057);
#4856=VERTEX_POINT('',#16059);
#4857=VERTEX_POINT('',#16063);
#4858=VERTEX_POINT('',#16065);
#4859=VERTEX_POINT('',#16072);
#4860=VERTEX_POINT('',#16074);
#4861=VERTEX_POINT('',#16077);
#4862=VERTEX_POINT('',#16081);
#4863=VERTEX_POINT('',#16089);
#4864=VERTEX_POINT('',#16090);
#4865=VERTEX_POINT('',#16092);
#4866=VERTEX_POINT('',#16094);
#4867=VERTEX_POINT('',#16098);
#4868=VERTEX_POINT('',#16100);
#4869=VERTEX_POINT('',#16104);
#4870=VERTEX_POINT('',#16106);
#4871=VERTEX_POINT('',#16110);
#4872=VERTEX_POINT('',#16112);
#4873=VERTEX_POINT('',#16116);
#4874=VERTEX_POINT('',#16118);
#4875=VERTEX_POINT('',#16127);
#4876=VERTEX_POINT('',#16130);
#4877=VERTEX_POINT('',#16133);
#4878=VERTEX_POINT('',#16137);
#4879=VERTEX_POINT('',#16141);
#4880=VERTEX_POINT('',#16145);
#4881=VERTEX_POINT('',#16148);
#4882=VERTEX_POINT('',#16156);
#4883=VERTEX_POINT('',#16158);
#4884=VERTEX_POINT('',#16163);
#4885=VERTEX_POINT('',#16165);
#4886=VERTEX_POINT('',#16170);
#4887=VERTEX_POINT('',#16172);
#4888=VERTEX_POINT('',#16175);
#4889=VERTEX_POINT('',#16177);
#4890=VERTEX_POINT('',#16182);
#4891=VERTEX_POINT('',#16186);
#4892=VERTEX_POINT('',#16189);
#4893=VERTEX_POINT('',#16191);
#4894=VERTEX_POINT('',#16196);
#4895=VERTEX_POINT('',#16200);
#4896=VERTEX_POINT('',#16207);
#4897=VERTEX_POINT('',#16209);
#4898=VERTEX_POINT('',#16213);
#4899=VERTEX_POINT('',#16215);
#4900=VERTEX_POINT('',#16222);
#4901=VERTEX_POINT('',#16224);
#4902=VERTEX_POINT('',#16228);
#4903=VERTEX_POINT('',#16230);
#4904=VERTEX_POINT('',#16237);
#4905=VERTEX_POINT('',#16239);
#4906=VERTEX_POINT('',#16243);
#4907=VERTEX_POINT('',#16244);
#4908=VERTEX_POINT('',#16248);
#4909=VERTEX_POINT('',#16249);
#4910=VERTEX_POINT('',#16256);
#4911=VERTEX_POINT('',#16258);
#4912=VERTEX_POINT('',#16277);
#4913=VERTEX_POINT('',#16279);
#4914=VERTEX_POINT('',#16290);
#4915=VERTEX_POINT('',#16322);
#4916=VERTEX_POINT('',#16325);
#4917=VERTEX_POINT('',#16328);
#4918=VERTEX_POINT('',#16332);
#4919=VERTEX_POINT('',#16340);
#4920=VERTEX_POINT('',#16342);
#4921=VERTEX_POINT('',#16346);
#4922=VERTEX_POINT('',#16348);
#4923=VERTEX_POINT('',#16355);
#4924=VERTEX_POINT('',#16357);
#4925=VERTEX_POINT('',#16361);
#4926=VERTEX_POINT('',#16363);
#4927=VERTEX_POINT('',#16370);
#4928=VERTEX_POINT('',#16371);
#4929=VERTEX_POINT('',#16375);
#4930=VERTEX_POINT('',#16376);
#4931=VERTEX_POINT('',#16385);
#4932=VERTEX_POINT('',#16387);
#4933=VERTEX_POINT('',#16412);
#4934=VERTEX_POINT('',#16414);
#4935=VERTEX_POINT('',#16425);
#4936=VERTEX_POINT('',#16457);
#4937=VERTEX_POINT('',#16460);
#4938=VERTEX_POINT('',#16464);
#4939=VERTEX_POINT('',#16467);
#4940=VERTEX_POINT('',#16474);
#4941=VERTEX_POINT('',#16477);
#4942=VERTEX_POINT('',#16481);
#4943=VERTEX_POINT('',#16485);
#4944=VERTEX_POINT('',#16489);
#4945=VERTEX_POINT('',#16492);
#4946=VERTEX_POINT('',#16496);
#4947=VERTEX_POINT('',#16500);
#4948=VERTEX_POINT('',#16505);
#4949=VERTEX_POINT('',#16506);
#4950=VERTEX_POINT('',#16508);
#4951=VERTEX_POINT('',#16510);
#4952=VERTEX_POINT('',#16514);
#4953=VERTEX_POINT('',#16516);
#4954=VERTEX_POINT('',#16520);
#4955=VERTEX_POINT('',#16522);
#4956=VERTEX_POINT('',#16526);
#4957=VERTEX_POINT('',#16528);
#4958=VERTEX_POINT('',#16532);
#4959=VERTEX_POINT('',#16534);
#4960=VERTEX_POINT('',#16586);
#4961=VERTEX_POINT('',#16587);
#4962=VERTEX_POINT('',#16589);
#4963=VERTEX_POINT('',#16591);
#4964=VERTEX_POINT('',#16595);
#4965=VERTEX_POINT('',#16597);
#4966=VERTEX_POINT('',#16601);
#4967=VERTEX_POINT('',#16603);
#4968=VERTEX_POINT('',#16607);
#4969=VERTEX_POINT('',#16609);
#4970=VERTEX_POINT('',#16613);
#4971=VERTEX_POINT('',#16615);
#4972=VERTEX_POINT('',#16623);
#4973=VERTEX_POINT('',#16626);
#4974=VERTEX_POINT('',#16630);
#4975=VERTEX_POINT('',#16634);
#4976=EDGE_CURVE('',#4233,#4233,#3723,.T.);
#4977=EDGE_CURVE('',#4233,#4234,#2577,.T.);
#4978=EDGE_CURVE('',#4234,#4234,#3724,.T.);
#4979=EDGE_CURVE('',#4235,#4235,#3725,.T.);
#4980=EDGE_CURVE('',#4235,#4236,#2578,.T.);
#4981=EDGE_CURVE('',#4236,#4236,#3726,.T.);
#4982=EDGE_CURVE('',#4237,#4237,#3727,.T.);
#4983=EDGE_CURVE('',#4237,#4238,#2579,.T.);
#4984=EDGE_CURVE('',#4238,#4238,#3728,.T.);
#4985=EDGE_CURVE('',#4239,#4239,#3729,.T.);
#4986=EDGE_CURVE('',#4239,#4240,#2580,.T.);
#4987=EDGE_CURVE('',#4240,#4240,#3730,.T.);
#4988=EDGE_CURVE('',#4241,#4241,#3731,.T.);
#4989=EDGE_CURVE('',#4241,#4242,#2581,.T.);
#4990=EDGE_CURVE('',#4242,#4242,#3732,.T.);
#4991=EDGE_CURVE('',#4243,#4243,#3733,.T.);
#4992=EDGE_CURVE('',#4243,#4244,#2582,.T.);
#4993=EDGE_CURVE('',#4244,#4244,#3734,.T.);
#4994=EDGE_CURVE('',#4245,#4245,#3735,.T.);
#4995=EDGE_CURVE('',#4245,#4246,#2583,.T.);
#4996=EDGE_CURVE('',#4246,#4246,#3736,.T.);
#4997=EDGE_CURVE('',#4247,#4247,#3737,.T.);
#4998=EDGE_CURVE('',#4247,#4248,#2584,.T.);
#4999=EDGE_CURVE('',#4248,#4248,#3738,.T.);
#5000=EDGE_CURVE('',#4249,#4249,#3739,.T.);
#5001=EDGE_CURVE('',#4249,#4250,#2585,.T.);
#5002=EDGE_CURVE('',#4250,#4250,#3740,.T.);
#5003=EDGE_CURVE('',#4251,#4251,#3741,.T.);
#5004=EDGE_CURVE('',#4251,#4252,#2586,.T.);
#5005=EDGE_CURVE('',#4252,#4252,#3742,.T.);
#5006=EDGE_CURVE('',#4253,#4253,#3743,.T.);
#5007=EDGE_CURVE('',#4253,#4254,#2587,.T.);
#5008=EDGE_CURVE('',#4254,#4254,#3744,.T.);
#5009=EDGE_CURVE('',#4255,#4255,#3745,.T.);
#5010=EDGE_CURVE('',#4255,#4256,#2588,.T.);
#5011=EDGE_CURVE('',#4256,#4256,#3746,.T.);
#5012=EDGE_CURVE('',#4257,#4258,#2589,.T.);
#5013=EDGE_CURVE('',#4258,#4259,#2590,.T.);
#5014=EDGE_CURVE('',#4260,#4259,#2591,.T.);
#5015=EDGE_CURVE('',#4257,#4260,#2592,.T.);
#5016=EDGE_CURVE('',#4261,#4257,#2593,.T.);
#5017=EDGE_CURVE('',#4262,#4260,#2594,.T.);
#5018=EDGE_CURVE('',#4261,#4262,#2595,.T.);
#5019=EDGE_CURVE('',#4263,#4261,#2596,.T.);
#5020=EDGE_CURVE('',#4264,#4262,#2597,.T.);
#5021=EDGE_CURVE('',#4263,#4264,#2598,.T.);
#5022=EDGE_CURVE('',#4258,#4263,#2599,.T.);
#5023=EDGE_CURVE('',#4259,#4264,#2600,.T.);
#5024=EDGE_CURVE('',#4265,#4266,#2601,.T.);
#5025=EDGE_CURVE('',#4266,#4267,#2602,.T.);
#5026=EDGE_CURVE('',#4268,#4267,#2603,.T.);
#5027=EDGE_CURVE('',#4265,#4268,#2604,.T.);
#5028=EDGE_CURVE('',#4269,#4265,#2605,.T.);
#5029=EDGE_CURVE('',#4270,#4268,#2606,.T.);
#5030=EDGE_CURVE('',#4269,#4270,#2607,.T.);
#5031=EDGE_CURVE('',#4271,#4269,#2608,.T.);
#5032=EDGE_CURVE('',#4272,#4270,#2609,.T.);
#5033=EDGE_CURVE('',#4271,#4272,#2610,.T.);
#5034=EDGE_CURVE('',#4266,#4271,#2611,.T.);
#5035=EDGE_CURVE('',#4267,#4272,#2612,.T.);
#5036=EDGE_CURVE('',#4273,#4274,#2613,.T.);
#5037=EDGE_CURVE('',#4274,#4275,#2614,.T.);
#5038=EDGE_CURVE('',#4276,#4275,#2615,.T.);
#5039=EDGE_CURVE('',#4273,#4276,#2616,.T.);
#5040=EDGE_CURVE('',#4277,#4273,#2617,.T.);
#5041=EDGE_CURVE('',#4278,#4276,#2618,.T.);
#5042=EDGE_CURVE('',#4277,#4278,#2619,.T.);
#5043=EDGE_CURVE('',#4279,#4277,#2620,.T.);
#5044=EDGE_CURVE('',#4280,#4278,#2621,.T.);
#5045=EDGE_CURVE('',#4279,#4280,#2622,.T.);
#5046=EDGE_CURVE('',#4274,#4279,#2623,.T.);
#5047=EDGE_CURVE('',#4275,#4280,#2624,.T.);
#5048=EDGE_CURVE('',#4281,#4282,#2625,.T.);
#5049=EDGE_CURVE('',#4283,#4281,#3747,.T.);
#5050=EDGE_CURVE('',#4283,#4284,#2626,.T.);
#5051=EDGE_CURVE('',#4282,#4284,#3748,.T.);
#5052=EDGE_CURVE('',#4285,#4286,#2627,.T.);
#5053=EDGE_CURVE('',#4287,#4285,#3749,.T.);
#5054=EDGE_CURVE('',#4287,#4288,#2628,.T.);
#5055=EDGE_CURVE('',#4286,#4288,#3750,.T.);
#5056=EDGE_CURVE('',#4289,#4290,#2629,.T.);
#5057=EDGE_CURVE('',#4289,#4290,#3751,.T.);
#5058=EDGE_CURVE('',#4291,#4292,#498,.T.);
#5059=EDGE_CURVE('',#4293,#4291,#3752,.T.);
#5060=EDGE_CURVE('',#4294,#4293,#499,.T.);
#5061=EDGE_CURVE('',#4290,#4294,#500,.T.);
#5062=EDGE_CURVE('',#4292,#4289,#501,.T.);
#5063=EDGE_CURVE('',#4292,#4295,#2630,.T.);
#5064=EDGE_CURVE('',#4295,#4295,#3753,.T.);
#5065=EDGE_CURVE('',#4293,#4291,#2631,.T.);
#5066=EDGE_CURVE('',#4288,#4286,#3754,.T.);
#5067=EDGE_CURVE('',#4287,#4288,#2632,.T.);
#5068=EDGE_CURVE('',#4285,#4287,#3755,.T.);
#5069=EDGE_CURVE('',#4296,#4296,#3756,.T.);
#5070=EDGE_CURVE('',#4284,#4282,#3757,.T.);
#5071=EDGE_CURVE('',#4283,#4284,#2633,.T.);
#5072=EDGE_CURVE('',#4281,#4283,#3758,.T.);
#5073=EDGE_CURVE('',#4297,#4297,#3759,.T.);
#5074=EDGE_CURVE('',#4298,#4299,#2634,.T.);
#5075=EDGE_CURVE('',#4299,#4288,#2635,.T.);
#5076=EDGE_CURVE('',#4288,#4300,#2636,.T.);
#5077=EDGE_CURVE('',#4300,#4301,#2637,.T.);
#5078=EDGE_CURVE('',#4301,#4284,#2638,.T.);
#5079=EDGE_CURVE('',#4284,#4298,#2639,.T.);
#5080=EDGE_CURVE('',#4302,#4302,#3760,.T.);
#5081=EDGE_CURVE('',#4302,#4296,#2640,.T.);
#5082=EDGE_CURVE('',#4303,#4303,#3761,.T.);
#5083=EDGE_CURVE('',#4303,#4297,#2641,.T.);
#5084=EDGE_CURVE('',#4304,#4304,#3762,.T.);
#5085=EDGE_CURVE('',#4304,#4292,#2642,.T.);
#5086=EDGE_CURVE('',#4294,#4305,#2643,.T.);
#5087=EDGE_CURVE('',#4305,#4305,#3763,.T.);
#5088=EDGE_CURVE('',#4306,#4307,#2644,.T.);
#5089=EDGE_CURVE('',#4307,#4298,#2645,.T.);
#5090=EDGE_CURVE('',#4306,#4301,#2646,.T.);
#5091=EDGE_CURVE('',#4308,#4306,#2647,.T.);
#5092=EDGE_CURVE('',#4308,#4300,#2648,.T.);
#5093=EDGE_CURVE('',#4309,#4308,#2649,.T.);
#5094=EDGE_CURVE('',#4309,#4299,#2650,.T.);
#5095=EDGE_CURVE('',#4307,#4309,#2651,.T.);
#5096=EDGE_CURVE('',#4310,#4311,#2652,.T.);
#5097=EDGE_CURVE('',#4312,#4310,#3764,.T.);
#5098=EDGE_CURVE('',#4312,#4313,#2653,.T.);
#5099=EDGE_CURVE('',#4311,#4313,#3765,.T.);
#5100=EDGE_CURVE('',#4314,#4315,#2654,.T.);
#5101=EDGE_CURVE('',#4316,#4314,#3766,.T.);
#5102=EDGE_CURVE('',#4316,#4317,#2655,.T.);
#5103=EDGE_CURVE('',#4315,#4317,#3767,.T.);
#5104=EDGE_CURVE('',#4318,#4319,#2656,.T.);
#5105=EDGE_CURVE('',#4318,#4319,#3768,.T.);
#5106=EDGE_CURVE('',#4320,#4321,#502,.T.);
#5107=EDGE_CURVE('',#4322,#4320,#3769,.T.);
#5108=EDGE_CURVE('',#4323,#4322,#503,.T.);
#5109=EDGE_CURVE('',#4319,#4323,#504,.T.);
#5110=EDGE_CURVE('',#4321,#4318,#505,.T.);
#5111=EDGE_CURVE('',#4321,#4324,#2657,.T.);
#5112=EDGE_CURVE('',#4324,#4324,#3770,.T.);
#5113=EDGE_CURVE('',#4322,#4320,#2658,.T.);
#5114=EDGE_CURVE('',#4317,#4315,#3771,.T.);
#5115=EDGE_CURVE('',#4316,#4317,#2659,.T.);
#5116=EDGE_CURVE('',#4314,#4316,#3772,.T.);
#5117=EDGE_CURVE('',#4325,#4325,#3773,.T.);
#5118=EDGE_CURVE('',#4313,#4311,#3774,.T.);
#5119=EDGE_CURVE('',#4312,#4313,#2660,.T.);
#5120=EDGE_CURVE('',#4310,#4312,#3775,.T.);
#5121=EDGE_CURVE('',#4326,#4326,#3776,.T.);
#5122=EDGE_CURVE('',#4327,#4328,#2661,.T.);
#5123=EDGE_CURVE('',#4328,#4317,#2662,.T.);
#5124=EDGE_CURVE('',#4317,#4329,#2663,.T.);
#5125=EDGE_CURVE('',#4329,#4330,#2664,.T.);
#5126=EDGE_CURVE('',#4330,#4313,#2665,.T.);
#5127=EDGE_CURVE('',#4313,#4327,#2666,.T.);
#5128=EDGE_CURVE('',#4331,#4331,#3777,.T.);
#5129=EDGE_CURVE('',#4331,#4325,#2667,.T.);
#5130=EDGE_CURVE('',#4332,#4332,#3778,.T.);
#5131=EDGE_CURVE('',#4332,#4326,#2668,.T.);
#5132=EDGE_CURVE('',#4333,#4333,#3779,.T.);
#5133=EDGE_CURVE('',#4333,#4321,#2669,.T.);
#5134=EDGE_CURVE('',#4323,#4334,#2670,.T.);
#5135=EDGE_CURVE('',#4334,#4334,#3780,.T.);
#5136=EDGE_CURVE('',#4335,#4336,#2671,.T.);
#5137=EDGE_CURVE('',#4336,#4327,#2672,.T.);
#5138=EDGE_CURVE('',#4335,#4330,#2673,.T.);
#5139=EDGE_CURVE('',#4337,#4335,#2674,.T.);
#5140=EDGE_CURVE('',#4337,#4329,#2675,.T.);
#5141=EDGE_CURVE('',#4338,#4337,#2676,.T.);
#5142=EDGE_CURVE('',#4338,#4328,#2677,.T.);
#5143=EDGE_CURVE('',#4336,#4338,#2678,.T.);
#5144=EDGE_CURVE('',#4339,#4340,#2679,.T.);
#5145=EDGE_CURVE('',#4341,#4339,#3781,.T.);
#5146=EDGE_CURVE('',#4341,#4342,#2680,.T.);
#5147=EDGE_CURVE('',#4340,#4342,#3782,.T.);
#5148=EDGE_CURVE('',#4343,#4344,#2681,.T.);
#5149=EDGE_CURVE('',#4345,#4343,#3783,.T.);
#5150=EDGE_CURVE('',#4345,#4346,#2682,.T.);
#5151=EDGE_CURVE('',#4344,#4346,#3784,.T.);
#5152=EDGE_CURVE('',#4347,#4348,#2683,.T.);
#5153=EDGE_CURVE('',#4347,#4348,#3785,.T.);
#5154=EDGE_CURVE('',#4349,#4350,#506,.T.);
#5155=EDGE_CURVE('',#4351,#4349,#3786,.T.);
#5156=EDGE_CURVE('',#4352,#4351,#507,.T.);
#5157=EDGE_CURVE('',#4348,#4352,#508,.T.);
#5158=EDGE_CURVE('',#4350,#4347,#509,.T.);
#5159=EDGE_CURVE('',#4350,#4353,#2684,.T.);
#5160=EDGE_CURVE('',#4353,#4353,#3787,.T.);
#5161=EDGE_CURVE('',#4351,#4349,#2685,.T.);
#5162=EDGE_CURVE('',#4346,#4344,#3788,.T.);
#5163=EDGE_CURVE('',#4345,#4346,#2686,.T.);
#5164=EDGE_CURVE('',#4343,#4345,#3789,.T.);
#5165=EDGE_CURVE('',#4354,#4354,#3790,.T.);
#5166=EDGE_CURVE('',#4342,#4340,#3791,.T.);
#5167=EDGE_CURVE('',#4341,#4342,#2687,.T.);
#5168=EDGE_CURVE('',#4339,#4341,#3792,.T.);
#5169=EDGE_CURVE('',#4355,#4355,#3793,.T.);
#5170=EDGE_CURVE('',#4356,#4357,#2688,.T.);
#5171=EDGE_CURVE('',#4357,#4346,#2689,.T.);
#5172=EDGE_CURVE('',#4346,#4358,#2690,.T.);
#5173=EDGE_CURVE('',#4358,#4359,#2691,.T.);
#5174=EDGE_CURVE('',#4359,#4342,#2692,.T.);
#5175=EDGE_CURVE('',#4342,#4356,#2693,.T.);
#5176=EDGE_CURVE('',#4360,#4360,#3794,.T.);
#5177=EDGE_CURVE('',#4360,#4354,#2694,.T.);
#5178=EDGE_CURVE('',#4361,#4361,#3795,.T.);
#5179=EDGE_CURVE('',#4361,#4355,#2695,.T.);
#5180=EDGE_CURVE('',#4362,#4362,#3796,.T.);
#5181=EDGE_CURVE('',#4362,#4350,#2696,.T.);
#5182=EDGE_CURVE('',#4352,#4363,#2697,.T.);
#5183=EDGE_CURVE('',#4363,#4363,#3797,.T.);
#5184=EDGE_CURVE('',#4364,#4365,#2698,.T.);
#5185=EDGE_CURVE('',#4365,#4356,#2699,.T.);
#5186=EDGE_CURVE('',#4364,#4359,#2700,.T.);
#5187=EDGE_CURVE('',#4366,#4364,#2701,.T.);
#5188=EDGE_CURVE('',#4366,#4358,#2702,.T.);
#5189=EDGE_CURVE('',#4367,#4366,#2703,.T.);
#5190=EDGE_CURVE('',#4367,#4357,#2704,.T.);
#5191=EDGE_CURVE('',#4365,#4367,#2705,.T.);
#5192=EDGE_CURVE('',#4368,#4369,#2706,.T.);
#5193=EDGE_CURVE('',#4370,#4368,#3798,.T.);
#5194=EDGE_CURVE('',#4370,#4371,#2707,.T.);
#5195=EDGE_CURVE('',#4369,#4371,#3799,.T.);
#5196=EDGE_CURVE('',#4372,#4373,#2708,.T.);
#5197=EDGE_CURVE('',#4374,#4372,#3800,.T.);
#5198=EDGE_CURVE('',#4374,#4375,#2709,.T.);
#5199=EDGE_CURVE('',#4373,#4375,#3801,.T.);
#5200=EDGE_CURVE('',#4376,#4377,#2710,.T.);
#5201=EDGE_CURVE('',#4376,#4377,#3802,.T.);
#5202=EDGE_CURVE('',#4378,#4379,#510,.T.);
#5203=EDGE_CURVE('',#4380,#4378,#3803,.T.);
#5204=EDGE_CURVE('',#4381,#4380,#511,.T.);
#5205=EDGE_CURVE('',#4377,#4381,#512,.T.);
#5206=EDGE_CURVE('',#4379,#4376,#513,.T.);
#5207=EDGE_CURVE('',#4379,#4382,#2711,.T.);
#5208=EDGE_CURVE('',#4382,#4382,#3804,.T.);
#5209=EDGE_CURVE('',#4380,#4378,#2712,.T.);
#5210=EDGE_CURVE('',#4375,#4373,#3805,.T.);
#5211=EDGE_CURVE('',#4374,#4375,#2713,.T.);
#5212=EDGE_CURVE('',#4372,#4374,#3806,.T.);
#5213=EDGE_CURVE('',#4383,#4383,#3807,.T.);
#5214=EDGE_CURVE('',#4371,#4369,#3808,.T.);
#5215=EDGE_CURVE('',#4370,#4371,#2714,.T.);
#5216=EDGE_CURVE('',#4368,#4370,#3809,.T.);
#5217=EDGE_CURVE('',#4384,#4384,#3810,.T.);
#5218=EDGE_CURVE('',#4385,#4386,#2715,.T.);
#5219=EDGE_CURVE('',#4386,#4375,#2716,.T.);
#5220=EDGE_CURVE('',#4375,#4387,#2717,.T.);
#5221=EDGE_CURVE('',#4387,#4388,#2718,.T.);
#5222=EDGE_CURVE('',#4388,#4371,#2719,.T.);
#5223=EDGE_CURVE('',#4371,#4385,#2720,.T.);
#5224=EDGE_CURVE('',#4389,#4389,#3811,.T.);
#5225=EDGE_CURVE('',#4389,#4383,#2721,.T.);
#5226=EDGE_CURVE('',#4390,#4390,#3812,.T.);
#5227=EDGE_CURVE('',#4390,#4384,#2722,.T.);
#5228=EDGE_CURVE('',#4391,#4391,#3813,.T.);
#5229=EDGE_CURVE('',#4391,#4379,#2723,.T.);
#5230=EDGE_CURVE('',#4381,#4392,#2724,.T.);
#5231=EDGE_CURVE('',#4392,#4392,#3814,.T.);
#5232=EDGE_CURVE('',#4393,#4394,#2725,.T.);
#5233=EDGE_CURVE('',#4394,#4385,#2726,.T.);
#5234=EDGE_CURVE('',#4393,#4388,#2727,.T.);
#5235=EDGE_CURVE('',#4395,#4393,#2728,.T.);
#5236=EDGE_CURVE('',#4395,#4387,#2729,.T.);
#5237=EDGE_CURVE('',#4396,#4395,#2730,.T.);
#5238=EDGE_CURVE('',#4396,#4386,#2731,.T.);
#5239=EDGE_CURVE('',#4394,#4396,#2732,.T.);
#5240=EDGE_CURVE('',#4397,#4397,#3815,.T.);
#5241=EDGE_CURVE('',#4397,#4398,#2733,.T.);
#5242=EDGE_CURVE('',#4398,#4398,#3816,.T.);
#5243=EDGE_CURVE('',#4399,#4399,#3817,.T.);
#5244=EDGE_CURVE('',#4399,#4400,#2734,.T.);
#5245=EDGE_CURVE('',#4400,#4400,#3818,.T.);
#5246=EDGE_CURVE('',#4401,#4401,#3819,.T.);
#5247=EDGE_CURVE('',#4401,#4402,#2735,.T.);
#5248=EDGE_CURVE('',#4402,#4402,#3820,.T.);
#5249=EDGE_CURVE('',#4403,#4403,#3821,.T.);
#5250=EDGE_CURVE('',#4403,#4404,#2736,.T.);
#5251=EDGE_CURVE('',#4404,#4404,#3822,.T.);
#5252=EDGE_CURVE('',#4405,#4405,#3823,.T.);
#5253=EDGE_CURVE('',#4405,#4406,#2737,.T.);
#5254=EDGE_CURVE('',#4406,#4406,#3824,.T.);
#5255=EDGE_CURVE('',#4407,#4407,#3825,.T.);
#5256=EDGE_CURVE('',#4407,#4408,#2738,.T.);
#5257=EDGE_CURVE('',#4408,#4408,#3826,.T.);
#5258=EDGE_CURVE('',#4409,#4409,#3827,.T.);
#5259=EDGE_CURVE('',#4409,#4410,#2739,.T.);
#5260=EDGE_CURVE('',#4410,#4410,#3828,.T.);
#5261=EDGE_CURVE('',#4411,#4412,#2740,.T.);
#5262=EDGE_CURVE('',#4413,#4411,#2741,.T.);
#5263=EDGE_CURVE('',#4414,#4413,#2742,.T.);
#5264=EDGE_CURVE('',#4414,#4412,#2743,.T.);
#5265=EDGE_CURVE('',#4415,#4416,#2744,.T.);
#5266=EDGE_CURVE('',#4415,#4417,#2745,.T.);
#5267=EDGE_CURVE('',#4417,#4418,#2746,.T.);
#5268=EDGE_CURVE('',#4416,#4418,#2747,.T.);
#5269=EDGE_CURVE('',#4419,#4414,#2748,.T.);
#5270=EDGE_CURVE('',#4420,#4413,#2749,.T.);
#5271=EDGE_CURVE('',#4419,#4420,#2750,.T.);
#5272=EDGE_CURVE('',#4417,#4421,#2751,.T.);
#5273=EDGE_CURVE('',#4421,#4422,#2752,.T.);
#5274=EDGE_CURVE('',#4418,#4422,#2753,.T.);
#5275=EDGE_CURVE('',#4416,#4423,#2754,.T.);
#5276=EDGE_CURVE('',#4424,#4423,#2755,.T.);
#5277=EDGE_CURVE('',#4415,#4424,#2756,.T.);
#5278=EDGE_CURVE('',#4411,#4425,#2757,.T.);
#5279=EDGE_CURVE('',#4423,#4425,#2758,.T.);
#5280=EDGE_CURVE('',#4422,#4420,#2759,.T.);
#5281=EDGE_CURVE('',#4412,#4426,#2760,.T.);
#5282=EDGE_CURVE('',#4425,#4426,#2761,.T.);
#5283=EDGE_CURVE('',#4426,#4424,#2762,.T.);
#5284=EDGE_CURVE('',#4419,#4421,#2763,.T.);
#5285=EDGE_CURVE('',#4427,#4427,#3829,.T.);
#5286=EDGE_CURVE('',#4427,#4428,#2764,.T.);
#5287=EDGE_CURVE('',#4428,#4428,#3830,.T.);
#5288=EDGE_CURVE('',#4429,#4429,#3831,.T.);
#5289=EDGE_CURVE('',#4429,#4430,#2765,.T.);
#5290=EDGE_CURVE('',#4430,#4430,#3832,.T.);
#5291=EDGE_CURVE('',#4431,#4431,#3833,.T.);
#5292=EDGE_CURVE('',#4431,#4432,#2766,.T.);
#5293=EDGE_CURVE('',#4432,#4432,#3834,.T.);
#5294=EDGE_CURVE('',#4433,#4433,#3835,.T.);
#5295=EDGE_CURVE('',#4433,#4434,#2767,.T.);
#5296=EDGE_CURVE('',#4434,#4434,#3836,.T.);
#5297=EDGE_CURVE('',#4435,#4435,#3837,.T.);
#5298=EDGE_CURVE('',#4435,#4436,#2768,.T.);
#5299=EDGE_CURVE('',#4436,#4436,#3838,.T.);
#5300=EDGE_CURVE('',#4437,#4437,#3839,.T.);
#5301=EDGE_CURVE('',#4437,#4438,#2769,.T.);
#5302=EDGE_CURVE('',#4438,#4438,#3840,.T.);
#5303=EDGE_CURVE('',#4439,#4439,#3841,.T.);
#5304=EDGE_CURVE('',#4439,#4440,#2770,.T.);
#5305=EDGE_CURVE('',#4440,#4440,#3842,.T.);
#5306=EDGE_CURVE('',#4441,#4441,#3843,.T.);
#5307=EDGE_CURVE('',#4441,#4442,#2771,.T.);
#5308=EDGE_CURVE('',#4442,#4442,#3844,.T.);
#5309=EDGE_CURVE('',#4443,#4443,#3845,.T.);
#5310=EDGE_CURVE('',#4443,#4444,#2772,.T.);
#5311=EDGE_CURVE('',#4444,#4444,#3846,.T.);
#5312=EDGE_CURVE('',#4445,#4445,#3847,.T.);
#5313=EDGE_CURVE('',#4445,#4446,#2773,.T.);
#5314=EDGE_CURVE('',#4446,#4446,#3848,.T.);
#5315=EDGE_CURVE('',#4447,#4447,#3849,.T.);
#5316=EDGE_CURVE('',#4447,#4448,#2774,.T.);
#5317=EDGE_CURVE('',#4448,#4448,#3850,.T.);
#5318=EDGE_CURVE('',#4449,#4449,#3851,.T.);
#5319=EDGE_CURVE('',#4449,#4450,#2775,.T.);
#5320=EDGE_CURVE('',#4450,#4450,#3852,.T.);
#5321=EDGE_CURVE('',#4451,#4451,#3853,.T.);
#5322=EDGE_CURVE('',#4452,#4452,#3854,.T.);
#5323=EDGE_CURVE('',#4452,#4451,#2776,.T.);
#5324=EDGE_CURVE('',#4453,#4453,#3855,.T.);
#5325=EDGE_CURVE('',#4453,#4454,#2777,.T.);
#5326=EDGE_CURVE('',#4454,#4454,#3856,.T.);
#5327=EDGE_CURVE('',#4455,#4455,#3857,.T.);
#5328=EDGE_CURVE('',#4455,#4456,#2778,.T.);
#5329=EDGE_CURVE('',#4456,#4456,#3858,.T.);
#5330=EDGE_CURVE('',#4457,#4457,#3859,.T.);
#5331=EDGE_CURVE('',#4457,#4458,#2779,.T.);
#5332=EDGE_CURVE('',#4458,#4458,#3860,.T.);
#5333=EDGE_CURVE('',#4459,#4459,#3861,.T.);
#5334=EDGE_CURVE('',#4459,#4460,#2780,.T.);
#5335=EDGE_CURVE('',#4460,#4460,#3862,.T.);
#5336=EDGE_CURVE('',#4461,#4461,#3863,.T.);
#5337=EDGE_CURVE('',#4461,#4462,#2781,.T.);
#5338=EDGE_CURVE('',#4462,#4462,#3864,.T.);
#5339=EDGE_CURVE('',#4463,#4463,#3865,.T.);
#5340=EDGE_CURVE('',#4463,#4464,#2782,.T.);
#5341=EDGE_CURVE('',#4464,#4464,#3866,.T.);
#5342=EDGE_CURVE('',#4465,#4465,#3867,.T.);
#5343=EDGE_CURVE('',#4465,#4466,#2783,.T.);
#5344=EDGE_CURVE('',#4466,#4466,#3868,.T.);
#5345=EDGE_CURVE('',#4467,#4467,#3869,.T.);
#5346=EDGE_CURVE('',#4467,#4468,#2784,.T.);
#5347=EDGE_CURVE('',#4468,#4468,#3870,.T.);
#5348=EDGE_CURVE('',#4469,#4470,#2785,.T.);
#5349=EDGE_CURVE('',#4471,#4469,#2786,.T.);
#5350=EDGE_CURVE('',#4472,#4471,#2787,.T.);
#5351=EDGE_CURVE('',#4472,#4470,#2788,.T.);
#5352=EDGE_CURVE('',#4473,#4474,#2789,.T.);
#5353=EDGE_CURVE('',#4473,#4475,#2790,.T.);
#5354=EDGE_CURVE('',#4475,#4476,#2791,.T.);
#5355=EDGE_CURVE('',#4474,#4476,#2792,.T.);
#5356=EDGE_CURVE('',#4477,#4472,#2793,.T.);
#5357=EDGE_CURVE('',#4478,#4471,#2794,.T.);
#5358=EDGE_CURVE('',#4477,#4478,#2795,.T.);
#5359=EDGE_CURVE('',#4475,#4479,#2796,.T.);
#5360=EDGE_CURVE('',#4479,#4480,#2797,.T.);
#5361=EDGE_CURVE('',#4476,#4480,#2798,.T.);
#5362=EDGE_CURVE('',#4474,#4481,#2799,.T.);
#5363=EDGE_CURVE('',#4482,#4481,#2800,.T.);
#5364=EDGE_CURVE('',#4473,#4482,#2801,.T.);
#5365=EDGE_CURVE('',#4469,#4483,#2802,.T.);
#5366=EDGE_CURVE('',#4481,#4483,#2803,.T.);
#5367=EDGE_CURVE('',#4480,#4478,#2804,.T.);
#5368=EDGE_CURVE('',#4470,#4484,#2805,.T.);
#5369=EDGE_CURVE('',#4483,#4484,#2806,.T.);
#5370=EDGE_CURVE('',#4484,#4482,#2807,.T.);
#5371=EDGE_CURVE('',#4477,#4479,#2808,.T.);
#5372=EDGE_CURVE('',#4485,#4485,#3871,.T.);
#5373=EDGE_CURVE('',#4485,#4486,#2809,.T.);
#5374=EDGE_CURVE('',#4486,#4486,#3872,.T.);
#5375=EDGE_CURVE('',#4487,#4487,#3873,.T.);
#5376=EDGE_CURVE('',#4487,#4488,#2810,.T.);
#5377=EDGE_CURVE('',#4488,#4488,#3874,.T.);
#5378=EDGE_CURVE('',#4489,#4489,#3875,.T.);
#5379=EDGE_CURVE('',#4489,#4490,#2811,.T.);
#5380=EDGE_CURVE('',#4490,#4490,#3876,.T.);
#5381=EDGE_CURVE('',#4491,#4491,#3877,.T.);
#5382=EDGE_CURVE('',#4491,#4492,#2812,.T.);
#5383=EDGE_CURVE('',#4492,#4492,#3878,.T.);
#5384=EDGE_CURVE('',#4493,#4493,#3879,.T.);
#5385=EDGE_CURVE('',#4493,#4494,#2813,.T.);
#5386=EDGE_CURVE('',#4494,#4494,#3880,.T.);
#5387=EDGE_CURVE('',#4495,#4495,#3881,.T.);
#5388=EDGE_CURVE('',#4495,#4496,#2814,.T.);
#5389=EDGE_CURVE('',#4496,#4496,#3882,.T.);
#5390=EDGE_CURVE('',#4497,#4497,#3883,.T.);
#5391=EDGE_CURVE('',#4497,#4498,#2815,.T.);
#5392=EDGE_CURVE('',#4498,#4498,#3884,.T.);
#5393=EDGE_CURVE('',#4499,#4499,#3885,.T.);
#5394=EDGE_CURVE('',#4499,#4500,#2816,.T.);
#5395=EDGE_CURVE('',#4500,#4500,#3886,.T.);
#5396=EDGE_CURVE('',#4501,#4501,#3887,.T.);
#5397=EDGE_CURVE('',#4501,#4502,#2817,.T.);
#5398=EDGE_CURVE('',#4502,#4502,#3888,.T.);
#5399=EDGE_CURVE('',#4503,#4503,#3889,.T.);
#5400=EDGE_CURVE('',#4503,#4504,#2818,.T.);
#5401=EDGE_CURVE('',#4504,#4504,#3890,.T.);
#5402=EDGE_CURVE('',#4505,#4505,#3891,.T.);
#5403=EDGE_CURVE('',#4505,#4506,#2819,.T.);
#5404=EDGE_CURVE('',#4506,#4506,#3892,.T.);
#5405=EDGE_CURVE('',#4507,#4507,#3893,.T.);
#5406=EDGE_CURVE('',#4507,#4508,#2820,.T.);
#5407=EDGE_CURVE('',#4508,#4508,#3894,.T.);
#5408=EDGE_CURVE('',#4509,#4509,#3895,.T.);
#5409=EDGE_CURVE('',#4510,#4510,#3896,.T.);
#5410=EDGE_CURVE('',#4510,#4509,#2821,.T.);
#5411=EDGE_CURVE('',#4511,#4511,#3897,.T.);
#5412=EDGE_CURVE('',#4511,#4512,#2822,.T.);
#5413=EDGE_CURVE('',#4512,#4512,#3898,.T.);
#5414=EDGE_CURVE('',#4513,#4513,#3899,.T.);
#5415=EDGE_CURVE('',#4513,#4514,#2823,.T.);
#5416=EDGE_CURVE('',#4514,#4514,#3900,.T.);
#5417=EDGE_CURVE('',#4515,#4515,#3901,.T.);
#5418=EDGE_CURVE('',#4515,#4513,#2824,.T.);
#5419=EDGE_CURVE('',#4516,#4516,#3902,.T.);
#5420=EDGE_CURVE('',#4516,#4515,#2825,.T.);
#5421=EDGE_CURVE('',#4517,#4518,#3903,.T.);
#5422=EDGE_CURVE('',#4518,#4517,#3904,.T.);
#5423=EDGE_CURVE('',#4518,#4519,#3905,.T.);
#5424=EDGE_CURVE('',#4520,#4519,#3906,.T.);
#5425=EDGE_CURVE('',#4519,#4520,#3907,.T.);
#5426=EDGE_CURVE('',#4520,#4521,#2826,.T.);
#5427=EDGE_CURVE('',#4521,#4521,#3908,.T.);
#5428=EDGE_CURVE('',#4522,#4522,#3909,.T.);
#5429=EDGE_CURVE('',#4522,#4523,#2827,.T.);
#5430=EDGE_CURVE('',#4523,#4523,#3910,.T.);
#5431=EDGE_CURVE('',#4523,#4524,#2828,.T.);
#5432=EDGE_CURVE('',#4524,#4524,#3911,.T.);
#5433=EDGE_CURVE('',#4525,#4525,#3912,.T.);
#5434=EDGE_CURVE('',#4525,#4517,#2829,.T.);
#5435=EDGE_CURVE('',#4526,#4526,#3913,.T.);
#5436=EDGE_CURVE('',#4526,#4522,#2830,.T.);
#5437=EDGE_CURVE('',#4527,#4528,#3914,.T.);
#5438=EDGE_CURVE('',#4528,#4527,#3915,.T.);
#5439=EDGE_CURVE('',#4528,#4529,#3916,.T.);
#5440=EDGE_CURVE('',#4530,#4529,#3917,.T.);
#5441=EDGE_CURVE('',#4529,#4530,#3918,.T.);
#5442=EDGE_CURVE('',#4531,#4531,#3919,.T.);
#5443=EDGE_CURVE('',#4531,#4530,#2831,.T.);
#5444=EDGE_CURVE('',#4532,#4532,#3920,.T.);
#5445=EDGE_CURVE('',#4533,#4533,#3921,.T.);
#5446=EDGE_CURVE('',#4534,#4534,#3922,.T.);
#5447=EDGE_CURVE('',#4534,#4532,#2832,.T.);
#5448=EDGE_CURVE('',#4535,#4535,#3923,.T.);
#5449=EDGE_CURVE('',#4535,#4534,#2833,.T.);
#5450=EDGE_CURVE('',#4536,#4536,#3924,.T.);
#5451=EDGE_CURVE('',#4536,#4535,#2834,.T.);
#5452=EDGE_CURVE('',#4527,#4533,#2835,.T.);
#5453=EDGE_CURVE('',#4537,#4538,#3925,.T.);
#5454=EDGE_CURVE('',#4539,#4540,#3926,.T.);
#5455=EDGE_CURVE('',#4541,#4542,#3927,.T.);
#5456=EDGE_CURVE('',#4543,#4544,#3928,.T.);
#5457=EDGE_CURVE('',#4545,#4546,#3929,.T.);
#5458=EDGE_CURVE('',#4547,#4548,#3930,.T.);
#5459=EDGE_CURVE('',#4549,#4550,#3931,.T.);
#5460=EDGE_CURVE('',#4551,#4552,#514,.T.);
#5461=EDGE_CURVE('',#4553,#4551,#3932,.T.);
#5462=EDGE_CURVE('',#4554,#4553,#515,.T.);
#5463=EDGE_CURVE('',#4552,#4554,#3933,.T.);
#5464=EDGE_CURVE('',#4555,#4553,#3934,.T.);
#5465=EDGE_CURVE('',#4555,#4556,#516,.T.);
#5466=EDGE_CURVE('',#4557,#4556,#3935,.T.);
#5467=EDGE_CURVE('',#4557,#4558,#517,.T.);
#5468=EDGE_CURVE('',#4559,#4558,#3936,.T.);
#5469=EDGE_CURVE('',#4559,#4560,#2836,.T.);
#5470=EDGE_CURVE('',#4560,#4560,#3937,.T.);
#5471=EDGE_CURVE('',#4561,#4559,#3938,.T.);
#5472=EDGE_CURVE('',#4561,#4562,#518,.T.);
#5473=EDGE_CURVE('',#4563,#4562,#3939,.T.);
#5474=EDGE_CURVE('',#4563,#4564,#519,.T.);
#5475=EDGE_CURVE('',#4565,#4564,#3940,.T.);
#5476=EDGE_CURVE('',#4565,#4566,#520,.T.);
#5477=EDGE_CURVE('',#4567,#4566,#3941,.T.);
#5478=EDGE_CURVE('',#4567,#4568,#521,.T.);
#5479=EDGE_CURVE('',#4554,#4568,#3942,.T.);
#5480=EDGE_CURVE('',#4551,#4569,#3943,.T.);
#5481=EDGE_CURVE('',#4569,#4555,#3944,.T.);
#5482=EDGE_CURVE('',#4570,#4569,#522,.T.);
#5483=EDGE_CURVE('',#4556,#4570,#3945,.T.);
#5484=EDGE_CURVE('',#4570,#4571,#3946,.T.);
#5485=EDGE_CURVE('',#4571,#4557,#3947,.T.);
#5486=EDGE_CURVE('',#4572,#4571,#523,.T.);
#5487=EDGE_CURVE('',#4558,#4572,#3948,.T.);
#5488=EDGE_CURVE('',#4572,#4573,#3949,.T.);
#5489=EDGE_CURVE('',#4573,#4574,#3950,.T.);
#5490=EDGE_CURVE('',#4574,#4561,#3951,.T.);
#5491=EDGE_CURVE('',#4575,#4574,#524,.T.);
#5492=EDGE_CURVE('',#4562,#4575,#3952,.T.);
#5493=EDGE_CURVE('',#4575,#4576,#3953,.T.);
#5494=EDGE_CURVE('',#4576,#4563,#3954,.T.);
#5495=EDGE_CURVE('',#4577,#4576,#525,.T.);
#5496=EDGE_CURVE('',#4564,#4577,#3955,.T.);
#5497=EDGE_CURVE('',#4577,#4578,#3956,.T.);
#5498=EDGE_CURVE('',#4578,#4565,#3957,.T.);
#5499=EDGE_CURVE('',#4579,#4578,#526,.T.);
#5500=EDGE_CURVE('',#4566,#4579,#3958,.T.);
#5501=EDGE_CURVE('',#4580,#4580,#3959,.T.);
#5502=EDGE_CURVE('',#4580,#4573,#2837,.T.);
#5503=EDGE_CURVE('',#4581,#4552,#3960,.T.);
#5504=EDGE_CURVE('',#4581,#4582,#527,.T.);
#5505=EDGE_CURVE('',#4579,#4582,#3961,.T.);
#5506=EDGE_CURVE('',#4568,#4581,#3962,.T.);
#5507=EDGE_CURVE('',#4582,#4567,#3963,.T.);
#5508=EDGE_CURVE('',#4583,#4583,#3964,.T.);
#5509=EDGE_CURVE('',#4584,#4584,#3965,.T.);
#5510=EDGE_CURVE('',#4585,#4585,#3966,.T.);
#5511=EDGE_CURVE('',#4585,#4583,#2838,.T.);
#5512=EDGE_CURVE('',#4586,#4586,#3967,.T.);
#5513=EDGE_CURVE('',#4586,#4584,#2839,.T.);
#5514=EDGE_CURVE('',#4587,#4587,#3968,.T.);
#5515=EDGE_CURVE('',#4588,#4588,#3969,.T.);
#5516=EDGE_CURVE('',#4589,#4589,#3970,.T.);
#5517=EDGE_CURVE('',#4589,#4587,#2840,.T.);
#5518=EDGE_CURVE('',#4590,#4590,#3971,.T.);
#5519=EDGE_CURVE('',#4590,#4588,#2841,.T.);
#5520=EDGE_CURVE('',#4591,#4591,#3972,.T.);
#5521=EDGE_CURVE('',#4591,#4592,#2842,.T.);
#5522=EDGE_CURVE('',#4592,#4592,#3973,.T.);
#5523=EDGE_CURVE('',#4593,#4593,#3974,.T.);
#5524=EDGE_CURVE('',#4593,#4594,#2843,.T.);
#5525=EDGE_CURVE('',#4594,#4594,#3975,.T.);
#5526=EDGE_CURVE('',#4595,#4595,#3976,.T.);
#5527=EDGE_CURVE('',#4595,#4596,#2844,.T.);
#5528=EDGE_CURVE('',#4596,#4596,#3977,.T.);
#5529=EDGE_CURVE('',#4597,#4597,#3978,.T.);
#5530=EDGE_CURVE('',#4597,#4598,#2845,.T.);
#5531=EDGE_CURVE('',#4598,#4598,#3979,.T.);
#5532=EDGE_CURVE('',#4599,#4599,#3980,.T.);
#5533=EDGE_CURVE('',#4599,#4600,#2846,.T.);
#5534=EDGE_CURVE('',#4600,#4600,#3981,.T.);
#5535=EDGE_CURVE('',#4601,#4601,#3982,.T.);
#5536=EDGE_CURVE('',#4601,#4602,#2847,.T.);
#5537=EDGE_CURVE('',#4602,#4602,#3983,.T.);
#5538=EDGE_CURVE('',#4603,#4603,#3984,.T.);
#5539=EDGE_CURVE('',#4603,#4604,#2848,.T.);
#5540=EDGE_CURVE('',#4604,#4604,#3985,.T.);
#5541=EDGE_CURVE('',#4605,#4605,#3986,.T.);
#5542=EDGE_CURVE('',#4605,#4606,#2849,.T.);
#5543=EDGE_CURVE('',#4606,#4606,#3987,.T.);
#5544=EDGE_CURVE('',#4607,#4607,#3988,.T.);
#5545=EDGE_CURVE('',#4607,#4608,#2850,.T.);
#5546=EDGE_CURVE('',#4608,#4608,#3989,.T.);
#5547=EDGE_CURVE('',#4609,#4609,#3990,.T.);
#5548=EDGE_CURVE('',#4609,#4610,#2851,.T.);
#5549=EDGE_CURVE('',#4610,#4610,#3991,.T.);
#5550=EDGE_CURVE('',#4611,#4611,#3992,.T.);
#5551=EDGE_CURVE('',#4611,#4612,#2852,.T.);
#5552=EDGE_CURVE('',#4612,#4612,#3993,.T.);
#5553=EDGE_CURVE('',#4613,#4613,#3994,.T.);
#5554=EDGE_CURVE('',#4613,#4614,#2853,.T.);
#5555=EDGE_CURVE('',#4614,#4614,#3995,.T.);
#5556=EDGE_CURVE('',#4615,#4615,#3996,.T.);
#5557=EDGE_CURVE('',#4615,#4616,#2854,.T.);
#5558=EDGE_CURVE('',#4616,#4616,#3997,.T.);
#5559=EDGE_CURVE('',#4617,#4618,#2855,.T.);
#5560=EDGE_CURVE('',#4618,#4619,#2856,.T.);
#5561=EDGE_CURVE('',#4620,#4619,#2857,.T.);
#5562=EDGE_CURVE('',#4617,#4620,#2858,.T.);
#5563=EDGE_CURVE('',#4621,#4617,#2859,.T.);
#5564=EDGE_CURVE('',#4622,#4620,#2860,.T.);
#5565=EDGE_CURVE('',#4621,#4622,#2861,.T.);
#5566=EDGE_CURVE('',#4623,#4621,#2862,.T.);
#5567=EDGE_CURVE('',#4624,#4622,#2863,.T.);
#5568=EDGE_CURVE('',#4623,#4624,#2864,.T.);
#5569=EDGE_CURVE('',#4618,#4623,#2865,.T.);
#5570=EDGE_CURVE('',#4619,#4624,#2866,.T.);
#5571=EDGE_CURVE('',#4625,#4625,#3998,.T.);
#5572=EDGE_CURVE('',#4625,#4626,#2867,.T.);
#5573=EDGE_CURVE('',#4626,#4626,#3999,.T.);
#5574=EDGE_CURVE('',#4627,#4627,#4000,.T.);
#5575=EDGE_CURVE('',#4627,#4628,#2868,.T.);
#5576=EDGE_CURVE('',#4628,#4628,#4001,.T.);
#5577=EDGE_CURVE('',#4629,#4629,#4002,.T.);
#5578=EDGE_CURVE('',#4629,#4630,#2869,.T.);
#5579=EDGE_CURVE('',#4630,#4630,#4003,.T.);
#5580=EDGE_CURVE('',#4631,#4631,#4004,.T.);
#5581=EDGE_CURVE('',#4631,#4632,#2870,.T.);
#5582=EDGE_CURVE('',#4632,#4632,#4005,.T.);
#5583=EDGE_CURVE('',#4633,#4633,#4006,.T.);
#5584=EDGE_CURVE('',#4633,#4634,#2871,.T.);
#5585=EDGE_CURVE('',#4634,#4634,#4007,.T.);
#5586=EDGE_CURVE('',#4635,#4635,#4008,.T.);
#5587=EDGE_CURVE('',#4635,#4636,#2872,.T.);
#5588=EDGE_CURVE('',#4636,#4636,#4009,.T.);
#5589=EDGE_CURVE('',#4637,#4637,#4010,.T.);
#5590=EDGE_CURVE('',#4637,#4638,#2873,.T.);
#5591=EDGE_CURVE('',#4638,#4638,#4011,.T.);
#5592=EDGE_CURVE('',#4639,#4640,#2874,.T.);
#5593=EDGE_CURVE('',#4640,#4641,#2875,.T.);
#5594=EDGE_CURVE('',#4642,#4641,#2876,.T.);
#5595=EDGE_CURVE('',#4639,#4642,#2877,.T.);
#5596=EDGE_CURVE('',#4643,#4639,#2878,.T.);
#5597=EDGE_CURVE('',#4644,#4642,#2879,.T.);
#5598=EDGE_CURVE('',#4643,#4644,#2880,.T.);
#5599=EDGE_CURVE('',#4645,#4643,#2881,.T.);
#5600=EDGE_CURVE('',#4646,#4644,#2882,.T.);
#5601=EDGE_CURVE('',#4645,#4646,#2883,.T.);
#5602=EDGE_CURVE('',#4640,#4645,#2884,.T.);
#5603=EDGE_CURVE('',#4641,#4646,#2885,.T.);
#5604=EDGE_CURVE('',#4647,#4647,#4012,.T.);
#5605=EDGE_CURVE('',#4647,#4648,#2886,.T.);
#5606=EDGE_CURVE('',#4648,#4648,#4013,.T.);
#5607=EDGE_CURVE('',#4649,#4649,#4014,.T.);
#5608=EDGE_CURVE('',#4649,#4650,#2887,.T.);
#5609=EDGE_CURVE('',#4650,#4650,#4015,.T.);
#5610=EDGE_CURVE('',#4651,#4651,#4016,.T.);
#5611=EDGE_CURVE('',#4651,#4652,#2888,.T.);
#5612=EDGE_CURVE('',#4652,#4652,#4017,.T.);
#5613=EDGE_CURVE('',#4653,#4653,#4018,.T.);
#5614=EDGE_CURVE('',#4653,#4654,#2889,.T.);
#5615=EDGE_CURVE('',#4654,#4654,#4019,.T.);
#5616=EDGE_CURVE('',#4655,#4655,#4020,.T.);
#5617=EDGE_CURVE('',#4655,#4656,#2890,.T.);
#5618=EDGE_CURVE('',#4656,#4656,#4021,.T.);
#5619=EDGE_CURVE('',#4657,#4657,#4022,.T.);
#5620=EDGE_CURVE('',#4657,#4658,#2891,.T.);
#5621=EDGE_CURVE('',#4658,#4658,#4023,.T.);
#5622=EDGE_CURVE('',#4659,#4659,#4024,.T.);
#5623=EDGE_CURVE('',#4659,#4660,#2892,.T.);
#5624=EDGE_CURVE('',#4660,#4660,#4025,.T.);
#5625=EDGE_CURVE('',#4661,#4662,#2893,.T.);
#5626=EDGE_CURVE('',#4662,#4663,#2894,.T.);
#5627=EDGE_CURVE('',#4664,#4663,#2895,.T.);
#5628=EDGE_CURVE('',#4661,#4664,#2896,.T.);
#5629=EDGE_CURVE('',#4665,#4661,#2897,.T.);
#5630=EDGE_CURVE('',#4666,#4664,#2898,.T.);
#5631=EDGE_CURVE('',#4665,#4666,#2899,.T.);
#5632=EDGE_CURVE('',#4667,#4665,#2900,.T.);
#5633=EDGE_CURVE('',#4668,#4666,#2901,.T.);
#5634=EDGE_CURVE('',#4667,#4668,#2902,.T.);
#5635=EDGE_CURVE('',#4662,#4667,#2903,.T.);
#5636=EDGE_CURVE('',#4663,#4668,#2904,.T.);
#5637=EDGE_CURVE('',#4669,#4670,#4026,.T.);
#5638=EDGE_CURVE('',#4669,#4671,#4027,.T.);
#5639=EDGE_CURVE('',#4671,#4670,#4028,.T.);
#5640=EDGE_CURVE('',#4672,#4669,#2905,.T.);
#5641=EDGE_CURVE('',#4673,#4672,#4029,.T.);
#5642=EDGE_CURVE('',#4670,#4673,#2906,.T.);
#5643=EDGE_CURVE('',#4671,#4674,#2907,.T.);
#5644=EDGE_CURVE('',#4674,#4674,#4030,.T.);
#5645=EDGE_CURVE('',#4675,#4676,#4031,.T.);
#5646=EDGE_CURVE('',#4675,#4677,#4032,.T.);
#5647=EDGE_CURVE('',#4676,#4677,#4033,.T.);
#5648=EDGE_CURVE('',#4678,#4675,#2908,.T.);
#5649=EDGE_CURVE('',#4679,#4678,#4034,.T.);
#5650=EDGE_CURVE('',#4679,#4680,#2909,.T.);
#5651=EDGE_CURVE('',#4680,#4680,#4035,.T.);
#5652=EDGE_CURVE('',#4681,#4679,#4036,.T.);
#5653=EDGE_CURVE('',#4677,#4681,#2910,.T.);
#5654=EDGE_CURVE('',#4678,#4673,#4037,.T.);
#5655=EDGE_CURVE('',#4676,#4682,#2911,.T.);
#5656=EDGE_CURVE('',#4682,#4682,#4038,.T.);
#5657=EDGE_CURVE('',#4672,#4681,#4039,.T.);
#5658=EDGE_CURVE('',#4683,#4683,#4040,.T.);
#5659=EDGE_CURVE('',#4684,#4684,#4041,.T.);
#5660=EDGE_CURVE('',#4684,#4683,#2912,.T.);
#5661=EDGE_CURVE('',#4685,#4685,#4042,.T.);
#5662=EDGE_CURVE('',#4685,#4686,#2913,.T.);
#5663=EDGE_CURVE('',#4686,#4686,#4043,.T.);
#5664=EDGE_CURVE('',#4687,#4687,#4044,.T.);
#5665=EDGE_CURVE('',#4687,#4688,#2914,.T.);
#5666=EDGE_CURVE('',#4688,#4688,#4045,.T.);
#5667=EDGE_CURVE('',#4689,#4689,#4046,.T.);
#5668=EDGE_CURVE('',#4690,#4690,#4047,.T.);
#5669=EDGE_CURVE('',#4690,#4691,#2915,.T.);
#5670=EDGE_CURVE('',#4691,#4691,#4048,.T.);
#5671=EDGE_CURVE('',#4692,#4692,#4049,.T.);
#5672=EDGE_CURVE('',#4693,#4693,#4050,.T.);
#5673=EDGE_CURVE('',#4693,#4694,#2916,.T.);
#5674=EDGE_CURVE('',#4694,#4694,#4051,.T.);
#5675=EDGE_CURVE('',#4695,#4695,#4052,.T.);
#5676=EDGE_CURVE('',#4696,#4696,#4053,.T.);
#5677=EDGE_CURVE('',#4696,#4697,#2917,.T.);
#5678=EDGE_CURVE('',#4697,#4697,#4054,.T.);
#5679=EDGE_CURVE('',#4698,#4698,#4055,.T.);
#5680=EDGE_CURVE('',#4699,#4699,#4056,.T.);
#5681=EDGE_CURVE('',#4699,#4689,#2918,.T.);
#5682=EDGE_CURVE('',#4700,#4700,#4057,.T.);
#5683=EDGE_CURVE('',#4700,#4692,#2919,.T.);
#5684=EDGE_CURVE('',#4701,#4701,#4058,.T.);
#5685=EDGE_CURVE('',#4701,#4695,#2920,.T.);
#5686=EDGE_CURVE('',#4702,#4702,#4059,.T.);
#5687=EDGE_CURVE('',#4702,#4698,#2921,.T.);
#5688=EDGE_CURVE('',#4703,#4704,#2922,.T.);
#5689=EDGE_CURVE('',#4704,#4705,#2923,.T.);
#5690=EDGE_CURVE('',#4706,#4705,#2924,.T.);
#5691=EDGE_CURVE('',#4703,#4706,#2925,.T.);
#5692=EDGE_CURVE('',#4707,#4703,#2926,.T.);
#5693=EDGE_CURVE('',#4708,#4706,#2927,.T.);
#5694=EDGE_CURVE('',#4707,#4708,#2928,.T.);
#5695=EDGE_CURVE('',#4709,#4707,#2929,.T.);
#5696=EDGE_CURVE('',#4710,#4708,#2930,.T.);
#5697=EDGE_CURVE('',#4709,#4710,#2931,.T.);
#5698=EDGE_CURVE('',#4704,#4709,#2932,.T.);
#5699=EDGE_CURVE('',#4705,#4710,#2933,.T.);
#5700=EDGE_CURVE('',#4711,#4711,#4060,.T.);
#5701=EDGE_CURVE('',#4711,#4712,#2934,.T.);
#5702=EDGE_CURVE('',#4712,#4712,#4061,.T.);
#5703=EDGE_CURVE('',#4713,#4713,#4062,.T.);
#5704=EDGE_CURVE('',#4713,#4714,#2935,.T.);
#5705=EDGE_CURVE('',#4714,#4714,#4063,.T.);
#5706=EDGE_CURVE('',#4715,#4715,#4064,.T.);
#5707=EDGE_CURVE('',#4715,#4716,#2936,.T.);
#5708=EDGE_CURVE('',#4716,#4716,#4065,.T.);
#5709=EDGE_CURVE('',#4717,#4717,#4066,.T.);
#5710=EDGE_CURVE('',#4717,#4718,#2937,.T.);
#5711=EDGE_CURVE('',#4718,#4718,#4067,.T.);
#5712=EDGE_CURVE('',#4719,#4719,#4068,.T.);
#5713=EDGE_CURVE('',#4719,#4720,#2938,.T.);
#5714=EDGE_CURVE('',#4720,#4720,#4069,.T.);
#5715=EDGE_CURVE('',#4721,#4721,#4070,.T.);
#5716=EDGE_CURVE('',#4721,#4722,#2939,.T.);
#5717=EDGE_CURVE('',#4722,#4722,#4071,.T.);
#5718=EDGE_CURVE('',#4723,#4723,#4072,.T.);
#5719=EDGE_CURVE('',#4723,#4724,#2940,.T.);
#5720=EDGE_CURVE('',#4724,#4724,#4073,.T.);
#5721=EDGE_CURVE('',#4725,#4725,#4074,.T.);
#5722=EDGE_CURVE('',#4725,#4726,#2941,.T.);
#5723=EDGE_CURVE('',#4726,#4726,#4075,.T.);
#5724=EDGE_CURVE('',#4727,#4727,#4076,.T.);
#5725=EDGE_CURVE('',#4727,#4728,#2942,.T.);
#5726=EDGE_CURVE('',#4728,#4728,#4077,.T.);
#5727=EDGE_CURVE('',#4729,#4729,#4078,.T.);
#5728=EDGE_CURVE('',#4729,#4730,#2943,.T.);
#5729=EDGE_CURVE('',#4730,#4730,#4079,.T.);
#5730=EDGE_CURVE('',#4731,#4731,#4080,.T.);
#5731=EDGE_CURVE('',#4731,#4732,#2944,.T.);
#5732=EDGE_CURVE('',#4732,#4732,#4081,.T.);
#5733=EDGE_CURVE('',#4733,#4733,#4082,.T.);
#5734=EDGE_CURVE('',#4733,#4734,#2945,.T.);
#5735=EDGE_CURVE('',#4734,#4734,#4083,.T.);
#5736=EDGE_CURVE('',#4735,#4735,#4084,.T.);
#5737=EDGE_CURVE('',#4735,#4736,#2946,.T.);
#5738=EDGE_CURVE('',#4736,#4736,#4085,.T.);
#5739=EDGE_CURVE('',#4737,#4738,#2947,.T.);
#5740=EDGE_CURVE('',#4738,#4739,#2948,.T.);
#5741=EDGE_CURVE('',#4740,#4739,#2949,.T.);
#5742=EDGE_CURVE('',#4737,#4740,#2950,.T.);
#5743=EDGE_CURVE('',#4741,#4737,#2951,.T.);
#5744=EDGE_CURVE('',#4742,#4740,#2952,.T.);
#5745=EDGE_CURVE('',#4741,#4742,#2953,.T.);
#5746=EDGE_CURVE('',#4743,#4741,#2954,.T.);
#5747=EDGE_CURVE('',#4744,#4742,#2955,.T.);
#5748=EDGE_CURVE('',#4743,#4744,#2956,.T.);
#5749=EDGE_CURVE('',#4738,#4743,#2957,.T.);
#5750=EDGE_CURVE('',#4739,#4744,#2958,.T.);
#5751=EDGE_CURVE('',#4745,#4745,#4086,.T.);
#5752=EDGE_CURVE('',#4745,#4746,#2959,.T.);
#5753=EDGE_CURVE('',#4746,#4746,#4087,.T.);
#5754=EDGE_CURVE('',#4747,#4747,#4088,.T.);
#5755=EDGE_CURVE('',#4747,#4748,#2960,.T.);
#5756=EDGE_CURVE('',#4748,#4748,#4089,.T.);
#5757=EDGE_CURVE('',#4749,#4749,#4090,.T.);
#5758=EDGE_CURVE('',#4749,#4750,#2961,.T.);
#5759=EDGE_CURVE('',#4750,#4750,#4091,.T.);
#5760=EDGE_CURVE('',#4751,#4751,#4092,.T.);
#5761=EDGE_CURVE('',#4751,#4752,#2962,.T.);
#5762=EDGE_CURVE('',#4752,#4752,#4093,.T.);
#5763=EDGE_CURVE('',#4753,#4753,#4094,.T.);
#5764=EDGE_CURVE('',#4753,#4754,#2963,.T.);
#5765=EDGE_CURVE('',#4754,#4754,#4095,.T.);
#5766=EDGE_CURVE('',#4755,#4755,#4096,.T.);
#5767=EDGE_CURVE('',#4755,#4756,#2964,.T.);
#5768=EDGE_CURVE('',#4756,#4756,#4097,.T.);
#5769=EDGE_CURVE('',#4757,#4757,#4098,.T.);
#5770=EDGE_CURVE('',#4757,#4758,#2965,.T.);
#5771=EDGE_CURVE('',#4758,#4758,#4099,.T.);
#5772=EDGE_CURVE('',#4759,#4760,#2966,.T.);
#5773=EDGE_CURVE('',#4760,#4761,#2967,.T.);
#5774=EDGE_CURVE('',#4762,#4761,#2968,.T.);
#5775=EDGE_CURVE('',#4759,#4762,#2969,.T.);
#5776=EDGE_CURVE('',#4763,#4759,#2970,.T.);
#5777=EDGE_CURVE('',#4764,#4762,#2971,.T.);
#5778=EDGE_CURVE('',#4763,#4764,#2972,.T.);
#5779=EDGE_CURVE('',#4765,#4763,#2973,.T.);
#5780=EDGE_CURVE('',#4766,#4764,#2974,.T.);
#5781=EDGE_CURVE('',#4765,#4766,#2975,.T.);
#5782=EDGE_CURVE('',#4760,#4765,#2976,.T.);
#5783=EDGE_CURVE('',#4761,#4766,#2977,.T.);
#5784=EDGE_CURVE('',#4767,#4767,#4100,.T.);
#5785=EDGE_CURVE('',#4767,#4768,#2978,.T.);
#5786=EDGE_CURVE('',#4768,#4768,#4101,.T.);
#5787=EDGE_CURVE('',#4769,#4769,#4102,.T.);
#5788=EDGE_CURVE('',#4769,#4770,#2979,.T.);
#5789=EDGE_CURVE('',#4770,#4770,#4103,.T.);
#5790=EDGE_CURVE('',#4771,#4771,#4104,.T.);
#5791=EDGE_CURVE('',#4771,#4772,#2980,.T.);
#5792=EDGE_CURVE('',#4772,#4772,#4105,.T.);
#5793=EDGE_CURVE('',#4773,#4773,#4106,.T.);
#5794=EDGE_CURVE('',#4773,#4774,#2981,.T.);
#5795=EDGE_CURVE('',#4774,#4774,#4107,.T.);
#5796=EDGE_CURVE('',#4775,#4775,#4108,.T.);
#5797=EDGE_CURVE('',#4775,#4776,#2982,.T.);
#5798=EDGE_CURVE('',#4776,#4776,#4109,.T.);
#5799=EDGE_CURVE('',#4777,#4777,#4110,.T.);
#5800=EDGE_CURVE('',#4777,#4778,#2983,.T.);
#5801=EDGE_CURVE('',#4778,#4778,#4111,.T.);
#5802=EDGE_CURVE('',#4779,#4779,#4112,.T.);
#5803=EDGE_CURVE('',#4779,#4780,#2984,.T.);
#5804=EDGE_CURVE('',#4780,#4780,#4113,.T.);
#5805=EDGE_CURVE('',#4781,#4782,#2985,.T.);
#5806=EDGE_CURVE('',#4782,#4783,#2986,.T.);
#5807=EDGE_CURVE('',#4784,#4783,#2987,.T.);
#5808=EDGE_CURVE('',#4781,#4784,#2988,.T.);
#5809=EDGE_CURVE('',#4785,#4781,#2989,.T.);
#5810=EDGE_CURVE('',#4786,#4784,#2990,.T.);
#5811=EDGE_CURVE('',#4785,#4786,#2991,.T.);
#5812=EDGE_CURVE('',#4787,#4785,#2992,.T.);
#5813=EDGE_CURVE('',#4788,#4786,#2993,.T.);
#5814=EDGE_CURVE('',#4787,#4788,#2994,.T.);
#5815=EDGE_CURVE('',#4782,#4787,#2995,.T.);
#5816=EDGE_CURVE('',#4783,#4788,#2996,.T.);
#5817=EDGE_CURVE('',#4789,#4790,#4114,.T.);
#5818=EDGE_CURVE('',#4791,#4789,#4115,.T.);
#5819=EDGE_CURVE('',#4790,#4791,#4116,.T.);
#5820=EDGE_CURVE('',#4792,#4792,#4117,.T.);
#5821=EDGE_CURVE('',#4792,#4791,#2997,.T.);
#5822=EDGE_CURVE('',#4793,#4789,#2998,.T.);
#5823=EDGE_CURVE('',#4794,#4793,#4118,.T.);
#5824=EDGE_CURVE('',#4790,#4794,#2999,.T.);
#5825=EDGE_CURVE('',#4795,#4796,#4119,.T.);
#5826=EDGE_CURVE('',#4797,#4795,#4120,.T.);
#5827=EDGE_CURVE('',#4796,#4797,#4121,.T.);
#5828=EDGE_CURVE('',#4798,#4798,#4122,.T.);
#5829=EDGE_CURVE('',#4798,#4799,#3000,.T.);
#5830=EDGE_CURVE('',#4800,#4799,#4123,.T.);
#5831=EDGE_CURVE('',#4797,#4800,#3001,.T.);
#5832=EDGE_CURVE('',#4801,#4795,#3002,.T.);
#5833=EDGE_CURVE('',#4799,#4801,#4124,.T.);
#5834=EDGE_CURVE('',#4802,#4802,#4125,.T.);
#5835=EDGE_CURVE('',#4802,#4796,#3003,.T.);
#5836=EDGE_CURVE('',#4800,#4793,#4126,.T.);
#5837=EDGE_CURVE('',#4794,#4801,#4127,.T.);
#5838=EDGE_CURVE('',#4803,#4803,#4128,.T.);
#5839=EDGE_CURVE('',#4803,#4804,#3004,.T.);
#5840=EDGE_CURVE('',#4804,#4804,#4129,.T.);
#5841=EDGE_CURVE('',#4805,#4805,#4130,.T.);
#5842=EDGE_CURVE('',#4806,#4806,#4131,.T.);
#5843=EDGE_CURVE('',#4806,#4805,#3005,.T.);
#5844=EDGE_CURVE('',#4807,#4807,#4132,.T.);
#5845=EDGE_CURVE('',#4807,#4808,#3006,.T.);
#5846=EDGE_CURVE('',#4808,#4808,#4133,.T.);
#5847=EDGE_CURVE('',#4809,#4809,#4134,.T.);
#5848=EDGE_CURVE('',#4810,#4810,#4135,.T.);
#5849=EDGE_CURVE('',#4810,#4811,#3007,.T.);
#5850=EDGE_CURVE('',#4811,#4811,#4136,.T.);
#5851=EDGE_CURVE('',#4812,#4812,#4137,.T.);
#5852=EDGE_CURVE('',#4813,#4813,#4138,.T.);
#5853=EDGE_CURVE('',#4813,#4814,#3008,.T.);
#5854=EDGE_CURVE('',#4814,#4814,#4139,.T.);
#5855=EDGE_CURVE('',#4815,#4815,#4140,.T.);
#5856=EDGE_CURVE('',#4816,#4816,#4141,.T.);
#5857=EDGE_CURVE('',#4816,#4817,#3009,.T.);
#5858=EDGE_CURVE('',#4817,#4817,#4142,.T.);
#5859=EDGE_CURVE('',#4818,#4818,#4143,.T.);
#5860=EDGE_CURVE('',#4809,#4819,#3010,.T.);
#5861=EDGE_CURVE('',#4819,#4819,#4144,.T.);
#5862=EDGE_CURVE('',#4812,#4820,#3011,.T.);
#5863=EDGE_CURVE('',#4820,#4820,#4145,.T.);
#5864=EDGE_CURVE('',#4815,#4821,#3012,.T.);
#5865=EDGE_CURVE('',#4821,#4821,#4146,.T.);
#5866=EDGE_CURVE('',#4818,#4822,#3013,.T.);
#5867=EDGE_CURVE('',#4822,#4822,#4147,.T.);
#5868=EDGE_CURVE('',#4823,#4824,#3014,.T.);
#5869=EDGE_CURVE('',#4824,#4825,#3015,.T.);
#5870=EDGE_CURVE('',#4826,#4825,#3016,.T.);
#5871=EDGE_CURVE('',#4823,#4826,#3017,.T.);
#5872=EDGE_CURVE('',#4827,#4823,#3018,.T.);
#5873=EDGE_CURVE('',#4828,#4826,#3019,.T.);
#5874=EDGE_CURVE('',#4827,#4828,#3020,.T.);
#5875=EDGE_CURVE('',#4829,#4827,#3021,.T.);
#5876=EDGE_CURVE('',#4830,#4828,#3022,.T.);
#5877=EDGE_CURVE('',#4829,#4830,#3023,.T.);
#5878=EDGE_CURVE('',#4824,#4829,#3024,.T.);
#5879=EDGE_CURVE('',#4825,#4830,#3025,.T.);
#5880=EDGE_CURVE('',#4831,#4832,#4148,.T.);
#5881=EDGE_CURVE('',#4833,#4831,#3026,.T.);
#5882=EDGE_CURVE('',#4834,#4833,#3027,.T.);
#5883=EDGE_CURVE('',#4832,#4834,#3028,.T.);
#5884=EDGE_CURVE('',#4832,#4835,#3029,.T.);
#5885=EDGE_CURVE('',#4836,#4834,#3030,.T.);
#5886=EDGE_CURVE('',#4836,#4835,#3031,.T.);
#5887=EDGE_CURVE('',#4835,#4837,#4149,.T.);
#5888=EDGE_CURVE('',#4838,#4836,#3032,.T.);
#5889=EDGE_CURVE('',#4837,#4838,#3033,.T.);
#5890=EDGE_CURVE('',#4837,#4831,#3034,.T.);
#5891=EDGE_CURVE('',#4838,#4833,#3035,.T.);
#5892=EDGE_CURVE('',#4839,#4839,#4150,.T.);
#5893=EDGE_CURVE('',#4840,#4840,#4151,.T.);
#5894=EDGE_CURVE('',#4841,#4841,#4152,.T.);
#5895=EDGE_CURVE('',#4841,#4839,#3036,.T.);
#5896=EDGE_CURVE('',#4842,#4842,#4153,.T.);
#5897=EDGE_CURVE('',#4843,#4843,#4154,.T.);
#5898=EDGE_CURVE('',#4843,#4842,#3037,.T.);
#5899=EDGE_CURVE('',#4844,#4844,#4155,.T.);
#5900=EDGE_CURVE('',#4845,#4845,#4156,.T.);
#5901=EDGE_CURVE('',#4845,#4844,#3038,.T.);
#5902=EDGE_CURVE('',#4846,#4846,#4157,.T.);
#5903=EDGE_CURVE('',#4847,#4847,#4158,.T.);
#5904=EDGE_CURVE('',#4847,#4846,#3039,.T.);
#5905=EDGE_CURVE('',#4848,#4848,#4159,.T.);
#5906=EDGE_CURVE('',#4849,#4849,#4160,.T.);
#5907=EDGE_CURVE('',#4849,#4848,#3040,.T.);
#5908=EDGE_CURVE('',#4850,#4850,#4161,.T.);
#5909=EDGE_CURVE('',#4850,#4840,#3041,.T.);
#5910=EDGE_CURVE('',#4851,#4852,#4162,.T.);
#5911=EDGE_CURVE('',#4853,#4851,#3042,.T.);
#5912=EDGE_CURVE('',#4854,#4853,#4163,.T.);
#5913=EDGE_CURVE('',#4852,#4854,#3043,.T.);
#5914=EDGE_CURVE('',#4852,#4855,#3044,.T.);
#5915=EDGE_CURVE('',#4856,#4854,#3045,.T.);
#5916=EDGE_CURVE('',#4856,#4855,#3046,.T.);
#5917=EDGE_CURVE('',#4855,#4857,#4164,.T.);
#5918=EDGE_CURVE('',#4858,#4856,#4165,.T.);
#5919=EDGE_CURVE('',#4857,#4858,#3047,.T.);
#5920=EDGE_CURVE('',#4857,#4851,#3048,.T.);
#5921=EDGE_CURVE('',#4853,#4858,#3049,.T.);
#5922=EDGE_CURVE('',#4859,#4859,#4166,.T.);
#5923=EDGE_CURVE('',#4860,#4860,#4167,.T.);
#5924=EDGE_CURVE('',#4861,#4861,#4168,.T.);
#5925=EDGE_CURVE('',#4861,#4859,#3050,.T.);
#5926=EDGE_CURVE('',#4862,#4862,#4169,.T.);
#5927=EDGE_CURVE('',#4862,#4860,#3051,.T.);
#5928=EDGE_CURVE('',#4863,#4864,#3052,.T.);
#5929=EDGE_CURVE('',#4864,#4865,#3053,.T.);
#5930=EDGE_CURVE('',#4865,#4866,#3054,.T.);
#5931=EDGE_CURVE('',#4863,#4866,#3055,.T.);
#5932=EDGE_CURVE('',#4864,#4867,#3056,.T.);
#5933=EDGE_CURVE('',#4867,#4868,#3057,.T.);
#5934=EDGE_CURVE('',#4868,#4865,#3058,.T.);
#5935=EDGE_CURVE('',#4867,#4869,#3059,.T.);
#5936=EDGE_CURVE('',#4869,#4870,#3060,.T.);
#5937=EDGE_CURVE('',#4870,#4868,#3061,.T.);
#5938=EDGE_CURVE('',#4869,#4871,#3062,.T.);
#5939=EDGE_CURVE('',#4871,#4872,#3063,.T.);
#5940=EDGE_CURVE('',#4872,#4870,#3064,.T.);
#5941=EDGE_CURVE('',#4871,#4873,#3065,.T.);
#5942=EDGE_CURVE('',#4873,#4874,#3066,.T.);
#5943=EDGE_CURVE('',#4874,#4872,#3067,.T.);
#5944=EDGE_CURVE('',#4873,#4863,#3068,.T.);
#5945=EDGE_CURVE('',#4866,#4874,#3069,.T.);
#5946=EDGE_CURVE('',#4875,#4875,#4170,.T.);
#5947=EDGE_CURVE('',#4876,#4876,#4171,.T.);
#5948=EDGE_CURVE('',#4877,#4877,#4172,.T.);
#5949=EDGE_CURVE('',#4877,#4876,#3070,.T.);
#5950=EDGE_CURVE('',#4878,#4878,#4173,.T.);
#5951=EDGE_CURVE('',#4878,#4877,#3071,.T.);
#5952=EDGE_CURVE('',#4879,#4879,#4174,.T.);
#5953=EDGE_CURVE('',#4879,#4878,#3072,.T.);
#5954=EDGE_CURVE('',#4880,#4880,#4175,.T.);
#5955=EDGE_CURVE('',#4881,#4881,#4176,.F.);
#5956=EDGE_CURVE('',#4881,#4880,#3073,.T.);
#5957=EDGE_CURVE('',#4875,#4881,#3074,.T.);
#5958=EDGE_CURVE('',#4882,#4882,#4177,.T.);
#5959=EDGE_CURVE('',#4882,#4883,#3075,.T.);
#5960=EDGE_CURVE('',#4883,#4883,#4178,.T.);
#5961=EDGE_CURVE('',#4884,#4884,#4179,.T.);
#5962=EDGE_CURVE('',#4884,#4885,#3076,.T.);
#5963=EDGE_CURVE('',#4885,#4885,#4180,.T.);
#5964=EDGE_CURVE('',#4886,#4886,#4181,.T.);
#5965=EDGE_CURVE('',#4887,#4887,#4182,.T.);
#5966=EDGE_CURVE('',#4888,#4888,#4183,.T.);
#5967=EDGE_CURVE('',#4889,#4889,#4184,.T.);
#5968=EDGE_CURVE('',#4886,#4888,#3077,.T.);
#5969=EDGE_CURVE('',#4889,#4890,#3078,.T.);
#5970=EDGE_CURVE('',#4890,#4890,#4185,.T.);
#5971=EDGE_CURVE('',#4891,#4891,#4186,.T.);
#5972=EDGE_CURVE('',#4892,#4892,#4187,.T.);
#5973=EDGE_CURVE('',#4893,#4893,#4188,.T.);
#5974=EDGE_CURVE('',#4891,#4892,#3079,.T.);
#5975=EDGE_CURVE('',#4893,#4894,#3080,.T.);
#5976=EDGE_CURVE('',#4894,#4894,#4189,.T.);
#5977=EDGE_CURVE('',#4895,#4895,#4190,.T.);
#5978=EDGE_CURVE('',#4895,#4887,#3081,.T.);
#5979=EDGE_CURVE('',#4896,#4896,#4191,.T.);
#5980=EDGE_CURVE('',#4896,#4897,#3082,.T.);
#5981=EDGE_CURVE('',#4897,#4897,#4192,.T.);
#5982=EDGE_CURVE('',#4898,#4898,#4193,.T.);
#5983=EDGE_CURVE('',#4898,#4899,#3083,.T.);
#5984=EDGE_CURVE('',#4899,#4899,#4194,.T.);
#5985=EDGE_CURVE('',#4900,#4900,#4195,.T.);
#5986=EDGE_CURVE('',#4900,#4901,#3084,.T.);
#5987=EDGE_CURVE('',#4901,#4901,#4196,.T.);
#5988=EDGE_CURVE('',#4902,#4902,#4197,.T.);
#5989=EDGE_CURVE('',#4902,#4903,#3085,.T.);
#5990=EDGE_CURVE('',#4903,#4903,#4198,.T.);
#5991=EDGE_CURVE('',#4904,#4904,#4199,.T.);
#5992=EDGE_CURVE('',#4904,#4905,#3086,.T.);
#5993=EDGE_CURVE('',#4905,#4905,#4200,.T.);
#5994=EDGE_CURVE('',#4906,#4907,#3087,.T.);
#5995=EDGE_CURVE('',#4906,#4907,#4201,.T.);
#5996=EDGE_CURVE('',#4908,#4909,#528,.T.);
#5997=EDGE_CURVE('',#4910,#4908,#4202,.T.);
#5998=EDGE_CURVE('',#4911,#4910,#529,.T.);
#5999=EDGE_CURVE('',#4907,#4911,#530,.T.);
#6000=EDGE_CURVE('',#4909,#4906,#531,.T.);
#6001=EDGE_CURVE('',#4909,#4912,#3088,.T.);
#6002=EDGE_CURVE('',#4913,#4912,#532,.T.);
#6003=EDGE_CURVE('',#4914,#4913,#533,.T.);
#6004=EDGE_CURVE('',#4912,#4914,#534,.T.);
#6005=EDGE_CURVE('',#4910,#4908,#3089,.T.);
#6006=EDGE_CURVE('',#4915,#4915,#4203,.T.);
#6007=EDGE_CURVE('',#4916,#4916,#4204,.T.);
#6008=EDGE_CURVE('',#4916,#4911,#3090,.T.);
#6009=EDGE_CURVE('',#4909,#4917,#3091,.T.);
#6010=EDGE_CURVE('',#4917,#4917,#4205,.T.);
#6011=EDGE_CURVE('',#4918,#4918,#4206,.T.);
#6012=EDGE_CURVE('',#4918,#4914,#3092,.T.);
#6013=EDGE_CURVE('',#4912,#4915,#3093,.T.);
#6014=EDGE_CURVE('',#4919,#4919,#4207,.T.);
#6015=EDGE_CURVE('',#4919,#4920,#3094,.T.);
#6016=EDGE_CURVE('',#4920,#4920,#4208,.T.);
#6017=EDGE_CURVE('',#4921,#4921,#4209,.T.);
#6018=EDGE_CURVE('',#4921,#4922,#3095,.T.);
#6019=EDGE_CURVE('',#4922,#4922,#4210,.T.);
#6020=EDGE_CURVE('',#4923,#4923,#4211,.T.);
#6021=EDGE_CURVE('',#4923,#4924,#3096,.T.);
#6022=EDGE_CURVE('',#4924,#4924,#4212,.T.);
#6023=EDGE_CURVE('',#4925,#4925,#4213,.T.);
#6024=EDGE_CURVE('',#4925,#4926,#3097,.T.);
#6025=EDGE_CURVE('',#4926,#4926,#4214,.T.);
#6026=EDGE_CURVE('',#4927,#4928,#3098,.T.);
#6027=EDGE_CURVE('',#4927,#4928,#4215,.T.);
#6028=EDGE_CURVE('',#4929,#4930,#535,.T.);
#6029=EDGE_CURVE('',#4931,#4929,#4216,.T.);
#6030=EDGE_CURVE('',#4932,#4931,#536,.T.);
#6031=EDGE_CURVE('',#4928,#4932,#537,.T.);
#6032=EDGE_CURVE('',#4930,#4927,#538,.T.);
#6033=EDGE_CURVE('',#4930,#4933,#3099,.T.);
#6034=EDGE_CURVE('',#4934,#4933,#539,.T.);
#6035=EDGE_CURVE('',#4935,#4934,#540,.T.);
#6036=EDGE_CURVE('',#4933,#4935,#541,.T.);
#6037=EDGE_CURVE('',#4931,#4929,#3100,.T.);
#6038=EDGE_CURVE('',#4936,#4936,#4217,.T.);
#6039=EDGE_CURVE('',#4936,#4932,#3101,.T.);
#6040=EDGE_CURVE('',#4930,#4937,#3102,.T.);
#6041=EDGE_CURVE('',#4937,#4937,#4218,.T.);
#6042=EDGE_CURVE('',#4938,#4938,#4219,.T.);
#6043=EDGE_CURVE('',#4938,#4935,#3103,.T.);
#6044=EDGE_CURVE('',#4933,#4939,#3104,.T.);
#6045=EDGE_CURVE('',#4939,#4939,#4220,.T.);
#6046=EDGE_CURVE('',#4940,#4940,#4221,.T.);
#6047=EDGE_CURVE('',#4941,#4941,#4222,.T.);
#6048=EDGE_CURVE('',#4941,#4940,#3105,.T.);
#6049=EDGE_CURVE('',#4942,#4942,#4223,.T.);
#6050=EDGE_CURVE('',#4942,#4941,#3106,.T.);
#6051=EDGE_CURVE('',#4943,#4943,#4224,.T.);
#6052=EDGE_CURVE('',#4943,#4942,#3107,.T.);
#6053=EDGE_CURVE('',#4944,#4944,#4225,.T.);
#6054=EDGE_CURVE('',#4945,#4945,#4226,.F.);
#6055=EDGE_CURVE('',#4945,#4944,#3108,.T.);
#6056=EDGE_CURVE('',#4946,#4946,#4227,.F.);
#6057=EDGE_CURVE('',#4946,#4945,#3109,.T.);
#6058=EDGE_CURVE('',#4947,#4947,#4228,.T.);
#6059=EDGE_CURVE('',#4947,#4946,#3110,.T.);
#6060=EDGE_CURVE('',#4948,#4949,#3111,.T.);
#6061=EDGE_CURVE('',#4949,#4950,#3112,.T.);
#6062=EDGE_CURVE('',#4950,#4951,#3113,.T.);
#6063=EDGE_CURVE('',#4948,#4951,#3114,.T.);
#6064=EDGE_CURVE('',#4949,#4952,#3115,.T.);
#6065=EDGE_CURVE('',#4952,#4953,#3116,.T.);
#6066=EDGE_CURVE('',#4953,#4950,#3117,.T.);
#6067=EDGE_CURVE('',#4952,#4954,#3118,.T.);
#6068=EDGE_CURVE('',#4954,#4955,#3119,.T.);
#6069=EDGE_CURVE('',#4955,#4953,#3120,.T.);
#6070=EDGE_CURVE('',#4954,#4956,#3121,.T.);
#6071=EDGE_CURVE('',#4956,#4957,#3122,.T.);
#6072=EDGE_CURVE('',#4957,#4955,#3123,.T.);
#6073=EDGE_CURVE('',#4956,#4958,#3124,.T.);
#6074=EDGE_CURVE('',#4958,#4959,#3125,.T.);
#6075=EDGE_CURVE('',#4959,#4957,#3126,.T.);
#6076=EDGE_CURVE('',#4958,#4948,#3127,.T.);
#6077=EDGE_CURVE('',#4951,#4959,#3128,.T.);
#6078=EDGE_CURVE('',#4960,#4961,#3129,.T.);
#6079=EDGE_CURVE('',#4960,#4962,#3130,.T.);
#6080=EDGE_CURVE('',#4962,#4963,#3131,.T.);
#6081=EDGE_CURVE('',#4961,#4963,#3132,.T.);
#6082=EDGE_CURVE('',#4964,#4960,#3133,.T.);
#6083=EDGE_CURVE('',#4964,#4965,#3134,.T.);
#6084=EDGE_CURVE('',#4965,#4962,#3135,.T.);
#6085=EDGE_CURVE('',#4966,#4964,#3136,.T.);
#6086=EDGE_CURVE('',#4966,#4967,#3137,.T.);
#6087=EDGE_CURVE('',#4967,#4965,#3138,.T.);
#6088=EDGE_CURVE('',#4968,#4966,#3139,.T.);
#6089=EDGE_CURVE('',#4968,#4969,#3140,.T.);
#6090=EDGE_CURVE('',#4969,#4967,#3141,.T.);
#6091=EDGE_CURVE('',#4970,#4968,#3142,.T.);
#6092=EDGE_CURVE('',#4970,#4971,#3143,.T.);
#6093=EDGE_CURVE('',#4971,#4969,#3144,.T.);
#6094=EDGE_CURVE('',#4961,#4970,#3145,.T.);
#6095=EDGE_CURVE('',#4963,#4971,#3146,.T.);
#6096=EDGE_CURVE('',#4972,#4972,#4229,.T.);
#6097=EDGE_CURVE('',#4973,#4973,#4230,.T.);
#6098=EDGE_CURVE('',#4973,#4972,#3147,.T.);
#6099=EDGE_CURVE('',#4974,#4974,#4231,.F.);
#6100=EDGE_CURVE('',#4974,#4973,#3148,.T.);
#6101=EDGE_CURVE('',#4975,#4975,#4232,.T.);
#6102=EDGE_CURVE('',#4975,#4974,#3149,.T.);
#6103=ORIENTED_EDGE('',*,*,#4976,.F.);
#6104=ORIENTED_EDGE('',*,*,#4977,.T.);
#6105=ORIENTED_EDGE('',*,*,#4978,.F.);
#6106=ORIENTED_EDGE('',*,*,#4977,.F.);
#6107=ORIENTED_EDGE('',*,*,#4979,.F.);
#6108=ORIENTED_EDGE('',*,*,#4980,.T.);
#6109=ORIENTED_EDGE('',*,*,#4981,.F.);
#6110=ORIENTED_EDGE('',*,*,#4980,.F.);
#6111=ORIENTED_EDGE('',*,*,#4982,.F.);
#6112=ORIENTED_EDGE('',*,*,#4983,.T.);
#6113=ORIENTED_EDGE('',*,*,#4984,.F.);
#6114=ORIENTED_EDGE('',*,*,#4983,.F.);
#6115=ORIENTED_EDGE('',*,*,#4985,.F.);
#6116=ORIENTED_EDGE('',*,*,#4986,.T.);
#6117=ORIENTED_EDGE('',*,*,#4987,.F.);
#6118=ORIENTED_EDGE('',*,*,#4986,.F.);
#6119=ORIENTED_EDGE('',*,*,#4988,.F.);
#6120=ORIENTED_EDGE('',*,*,#4989,.T.);
#6121=ORIENTED_EDGE('',*,*,#4990,.F.);
#6122=ORIENTED_EDGE('',*,*,#4989,.F.);
#6123=ORIENTED_EDGE('',*,*,#4991,.F.);
#6124=ORIENTED_EDGE('',*,*,#4992,.T.);
#6125=ORIENTED_EDGE('',*,*,#4993,.F.);
#6126=ORIENTED_EDGE('',*,*,#4992,.F.);
#6127=ORIENTED_EDGE('',*,*,#4994,.F.);
#6128=ORIENTED_EDGE('',*,*,#4995,.T.);
#6129=ORIENTED_EDGE('',*,*,#4996,.F.);
#6130=ORIENTED_EDGE('',*,*,#4995,.F.);
#6131=ORIENTED_EDGE('',*,*,#4997,.F.);
#6132=ORIENTED_EDGE('',*,*,#4998,.T.);
#6133=ORIENTED_EDGE('',*,*,#4999,.F.);
#6134=ORIENTED_EDGE('',*,*,#4998,.F.);
#6135=ORIENTED_EDGE('',*,*,#5000,.F.);
#6136=ORIENTED_EDGE('',*,*,#5001,.T.);
#6137=ORIENTED_EDGE('',*,*,#5002,.F.);
#6138=ORIENTED_EDGE('',*,*,#5001,.F.);
#6139=ORIENTED_EDGE('',*,*,#5003,.F.);
#6140=ORIENTED_EDGE('',*,*,#5004,.T.);
#6141=ORIENTED_EDGE('',*,*,#5005,.F.);
#6142=ORIENTED_EDGE('',*,*,#5004,.F.);
#6143=ORIENTED_EDGE('',*,*,#5006,.F.);
#6144=ORIENTED_EDGE('',*,*,#5007,.T.);
#6145=ORIENTED_EDGE('',*,*,#5008,.F.);
#6146=ORIENTED_EDGE('',*,*,#5007,.F.);
#6147=ORIENTED_EDGE('',*,*,#5009,.F.);
#6148=ORIENTED_EDGE('',*,*,#5010,.T.);
#6149=ORIENTED_EDGE('',*,*,#5011,.F.);
#6150=ORIENTED_EDGE('',*,*,#5010,.F.);
#6151=ORIENTED_EDGE('',*,*,#5012,.T.);
#6152=ORIENTED_EDGE('',*,*,#5013,.T.);
#6153=ORIENTED_EDGE('',*,*,#5014,.F.);
#6154=ORIENTED_EDGE('',*,*,#5015,.F.);
#6155=ORIENTED_EDGE('',*,*,#5016,.T.);
#6156=ORIENTED_EDGE('',*,*,#5015,.T.);
#6157=ORIENTED_EDGE('',*,*,#5017,.F.);
#6158=ORIENTED_EDGE('',*,*,#5018,.F.);
#6159=ORIENTED_EDGE('',*,*,#5019,.T.);
#6160=ORIENTED_EDGE('',*,*,#5018,.T.);
#6161=ORIENTED_EDGE('',*,*,#5020,.F.);
#6162=ORIENTED_EDGE('',*,*,#5021,.F.);
#6163=ORIENTED_EDGE('',*,*,#5022,.T.);
#6164=ORIENTED_EDGE('',*,*,#5021,.T.);
#6165=ORIENTED_EDGE('',*,*,#5023,.F.);
#6166=ORIENTED_EDGE('',*,*,#5013,.F.);
#6167=ORIENTED_EDGE('',*,*,#5023,.T.);
#6168=ORIENTED_EDGE('',*,*,#5020,.T.);
#6169=ORIENTED_EDGE('',*,*,#5017,.T.);
#6170=ORIENTED_EDGE('',*,*,#5014,.T.);
#6171=ORIENTED_EDGE('',*,*,#4984,.T.);
#6172=ORIENTED_EDGE('',*,*,#4987,.T.);
#6173=ORIENTED_EDGE('',*,*,#5011,.T.);
#6174=ORIENTED_EDGE('',*,*,#5008,.T.);
#6175=ORIENTED_EDGE('',*,*,#5005,.T.);
#6176=ORIENTED_EDGE('',*,*,#5002,.T.);
#6177=ORIENTED_EDGE('',*,*,#4999,.T.);
#6178=ORIENTED_EDGE('',*,*,#4996,.T.);
#6179=ORIENTED_EDGE('',*,*,#4993,.T.);
#6180=ORIENTED_EDGE('',*,*,#4990,.T.);
#6181=ORIENTED_EDGE('',*,*,#4981,.T.);
#6182=ORIENTED_EDGE('',*,*,#4978,.T.);
#6183=ORIENTED_EDGE('',*,*,#5022,.F.);
#6184=ORIENTED_EDGE('',*,*,#5012,.F.);
#6185=ORIENTED_EDGE('',*,*,#5016,.F.);
#6186=ORIENTED_EDGE('',*,*,#5019,.F.);
#6187=ORIENTED_EDGE('',*,*,#4982,.T.);
#6188=ORIENTED_EDGE('',*,*,#4985,.T.);
#6189=ORIENTED_EDGE('',*,*,#5009,.T.);
#6190=ORIENTED_EDGE('',*,*,#5006,.T.);
#6191=ORIENTED_EDGE('',*,*,#5003,.T.);
#6192=ORIENTED_EDGE('',*,*,#5000,.T.);
#6193=ORIENTED_EDGE('',*,*,#4997,.T.);
#6194=ORIENTED_EDGE('',*,*,#4994,.T.);
#6195=ORIENTED_EDGE('',*,*,#4991,.T.);
#6196=ORIENTED_EDGE('',*,*,#4988,.T.);
#6197=ORIENTED_EDGE('',*,*,#4979,.T.);
#6198=ORIENTED_EDGE('',*,*,#4976,.T.);
#6199=ORIENTED_EDGE('',*,*,#5024,.T.);
#6200=ORIENTED_EDGE('',*,*,#5025,.T.);
#6201=ORIENTED_EDGE('',*,*,#5026,.F.);
#6202=ORIENTED_EDGE('',*,*,#5027,.F.);
#6203=ORIENTED_EDGE('',*,*,#5028,.T.);
#6204=ORIENTED_EDGE('',*,*,#5027,.T.);
#6205=ORIENTED_EDGE('',*,*,#5029,.F.);
#6206=ORIENTED_EDGE('',*,*,#5030,.F.);
#6207=ORIENTED_EDGE('',*,*,#5031,.T.);
#6208=ORIENTED_EDGE('',*,*,#5030,.T.);
#6209=ORIENTED_EDGE('',*,*,#5032,.F.);
#6210=ORIENTED_EDGE('',*,*,#5033,.F.);
#6211=ORIENTED_EDGE('',*,*,#5034,.T.);
#6212=ORIENTED_EDGE('',*,*,#5033,.T.);
#6213=ORIENTED_EDGE('',*,*,#5035,.F.);
#6214=ORIENTED_EDGE('',*,*,#5025,.F.);
#6215=ORIENTED_EDGE('',*,*,#5035,.T.);
#6216=ORIENTED_EDGE('',*,*,#5032,.T.);
#6217=ORIENTED_EDGE('',*,*,#5029,.T.);
#6218=ORIENTED_EDGE('',*,*,#5026,.T.);
#6219=ORIENTED_EDGE('',*,*,#5034,.F.);
#6220=ORIENTED_EDGE('',*,*,#5024,.F.);
#6221=ORIENTED_EDGE('',*,*,#5028,.F.);
#6222=ORIENTED_EDGE('',*,*,#5031,.F.);
#6223=ORIENTED_EDGE('',*,*,#5036,.T.);
#6224=ORIENTED_EDGE('',*,*,#5037,.T.);
#6225=ORIENTED_EDGE('',*,*,#5038,.F.);
#6226=ORIENTED_EDGE('',*,*,#5039,.F.);
#6227=ORIENTED_EDGE('',*,*,#5040,.T.);
#6228=ORIENTED_EDGE('',*,*,#5039,.T.);
#6229=ORIENTED_EDGE('',*,*,#5041,.F.);
#6230=ORIENTED_EDGE('',*,*,#5042,.F.);
#6231=ORIENTED_EDGE('',*,*,#5043,.T.);
#6232=ORIENTED_EDGE('',*,*,#5042,.T.);
#6233=ORIENTED_EDGE('',*,*,#5044,.F.);
#6234=ORIENTED_EDGE('',*,*,#5045,.F.);
#6235=ORIENTED_EDGE('',*,*,#5046,.T.);
#6236=ORIENTED_EDGE('',*,*,#5045,.T.);
#6237=ORIENTED_EDGE('',*,*,#5047,.F.);
#6238=ORIENTED_EDGE('',*,*,#5037,.F.);
#6239=ORIENTED_EDGE('',*,*,#5047,.T.);
#6240=ORIENTED_EDGE('',*,*,#5044,.T.);
#6241=ORIENTED_EDGE('',*,*,#5041,.T.);
#6242=ORIENTED_EDGE('',*,*,#5038,.T.);
#6243=ORIENTED_EDGE('',*,*,#5046,.F.);
#6244=ORIENTED_EDGE('',*,*,#5036,.F.);
#6245=ORIENTED_EDGE('',*,*,#5040,.F.);
#6246=ORIENTED_EDGE('',*,*,#5043,.F.);
#6247=ORIENTED_EDGE('',*,*,#5048,.F.);
#6248=ORIENTED_EDGE('',*,*,#5049,.F.);
#6249=ORIENTED_EDGE('',*,*,#5050,.T.);
#6250=ORIENTED_EDGE('',*,*,#5051,.F.);
#6251=ORIENTED_EDGE('',*,*,#5052,.F.);
#6252=ORIENTED_EDGE('',*,*,#5053,.F.);
#6253=ORIENTED_EDGE('',*,*,#5054,.T.);
#6254=ORIENTED_EDGE('',*,*,#5055,.F.);
#6255=ORIENTED_EDGE('',*,*,#5056,.F.);
#6256=ORIENTED_EDGE('',*,*,#5057,.T.);
#6257=ORIENTED_EDGE('',*,*,#5058,.F.);
#6258=ORIENTED_EDGE('',*,*,#5059,.F.);
#6259=ORIENTED_EDGE('',*,*,#5060,.F.);
#6260=ORIENTED_EDGE('',*,*,#5061,.F.);
#6261=ORIENTED_EDGE('',*,*,#5057,.F.);
#6262=ORIENTED_EDGE('',*,*,#5062,.F.);
#6263=ORIENTED_EDGE('',*,*,#5063,.T.);
#6264=ORIENTED_EDGE('',*,*,#5064,.F.);
#6265=ORIENTED_EDGE('',*,*,#5063,.F.);
#6266=ORIENTED_EDGE('',*,*,#5065,.F.);
#6267=ORIENTED_EDGE('',*,*,#5059,.T.);
#6268=ORIENTED_EDGE('',*,*,#5052,.T.);
#6269=ORIENTED_EDGE('',*,*,#5066,.F.);
#6270=ORIENTED_EDGE('',*,*,#5067,.F.);
#6271=ORIENTED_EDGE('',*,*,#5068,.F.);
#6272=ORIENTED_EDGE('',*,*,#5053,.T.);
#6273=ORIENTED_EDGE('',*,*,#5068,.T.);
#6274=ORIENTED_EDGE('',*,*,#5069,.F.);
#6275=ORIENTED_EDGE('',*,*,#5048,.T.);
#6276=ORIENTED_EDGE('',*,*,#5070,.F.);
#6277=ORIENTED_EDGE('',*,*,#5071,.F.);
#6278=ORIENTED_EDGE('',*,*,#5072,.F.);
#6279=ORIENTED_EDGE('',*,*,#5049,.T.);
#6280=ORIENTED_EDGE('',*,*,#5072,.T.);
#6281=ORIENTED_EDGE('',*,*,#5073,.F.);
#6282=ORIENTED_EDGE('',*,*,#5074,.T.);
#6283=ORIENTED_EDGE('',*,*,#5075,.T.);
#6284=ORIENTED_EDGE('',*,*,#5066,.T.);
#6285=ORIENTED_EDGE('',*,*,#5055,.T.);
#6286=ORIENTED_EDGE('',*,*,#5076,.T.);
#6287=ORIENTED_EDGE('',*,*,#5077,.T.);
#6288=ORIENTED_EDGE('',*,*,#5078,.T.);
#6289=ORIENTED_EDGE('',*,*,#5070,.T.);
#6290=ORIENTED_EDGE('',*,*,#5051,.T.);
#6291=ORIENTED_EDGE('',*,*,#5079,.T.);
#6292=ORIENTED_EDGE('',*,*,#5064,.T.);
#6293=ORIENTED_EDGE('',*,*,#5080,.F.);
#6294=ORIENTED_EDGE('',*,*,#5081,.T.);
#6295=ORIENTED_EDGE('',*,*,#5069,.T.);
#6296=ORIENTED_EDGE('',*,*,#5081,.F.);
#6297=ORIENTED_EDGE('',*,*,#5082,.F.);
#6298=ORIENTED_EDGE('',*,*,#5083,.T.);
#6299=ORIENTED_EDGE('',*,*,#5073,.T.);
#6300=ORIENTED_EDGE('',*,*,#5083,.F.);
#6301=ORIENTED_EDGE('',*,*,#5084,.F.);
#6302=ORIENTED_EDGE('',*,*,#5085,.T.);
#6303=ORIENTED_EDGE('',*,*,#5062,.T.);
#6304=ORIENTED_EDGE('',*,*,#5056,.T.);
#6305=ORIENTED_EDGE('',*,*,#5061,.T.);
#6306=ORIENTED_EDGE('',*,*,#5086,.T.);
#6307=ORIENTED_EDGE('',*,*,#5087,.F.);
#6308=ORIENTED_EDGE('',*,*,#5086,.F.);
#6309=ORIENTED_EDGE('',*,*,#5060,.T.);
#6310=ORIENTED_EDGE('',*,*,#5065,.T.);
#6311=ORIENTED_EDGE('',*,*,#5058,.T.);
#6312=ORIENTED_EDGE('',*,*,#5085,.F.);
#6313=ORIENTED_EDGE('',*,*,#5088,.T.);
#6314=ORIENTED_EDGE('',*,*,#5089,.T.);
#6315=ORIENTED_EDGE('',*,*,#5079,.F.);
#6316=ORIENTED_EDGE('',*,*,#5050,.F.);
#6317=ORIENTED_EDGE('',*,*,#5071,.T.);
#6318=ORIENTED_EDGE('',*,*,#5078,.F.);
#6319=ORIENTED_EDGE('',*,*,#5090,.F.);
#6320=ORIENTED_EDGE('',*,*,#5091,.T.);
#6321=ORIENTED_EDGE('',*,*,#5090,.T.);
#6322=ORIENTED_EDGE('',*,*,#5077,.F.);
#6323=ORIENTED_EDGE('',*,*,#5092,.F.);
#6324=ORIENTED_EDGE('',*,*,#5087,.T.);
#6325=ORIENTED_EDGE('',*,*,#5093,.T.);
#6326=ORIENTED_EDGE('',*,*,#5092,.T.);
#6327=ORIENTED_EDGE('',*,*,#5076,.F.);
#6328=ORIENTED_EDGE('',*,*,#5054,.F.);
#6329=ORIENTED_EDGE('',*,*,#5067,.T.);
#6330=ORIENTED_EDGE('',*,*,#5075,.F.);
#6331=ORIENTED_EDGE('',*,*,#5094,.F.);
#6332=ORIENTED_EDGE('',*,*,#5095,.T.);
#6333=ORIENTED_EDGE('',*,*,#5094,.T.);
#6334=ORIENTED_EDGE('',*,*,#5074,.F.);
#6335=ORIENTED_EDGE('',*,*,#5089,.F.);
#6336=ORIENTED_EDGE('',*,*,#5084,.T.);
#6337=ORIENTED_EDGE('',*,*,#5095,.F.);
#6338=ORIENTED_EDGE('',*,*,#5088,.F.);
#6339=ORIENTED_EDGE('',*,*,#5091,.F.);
#6340=ORIENTED_EDGE('',*,*,#5093,.F.);
#6341=ORIENTED_EDGE('',*,*,#5080,.T.);
#6342=ORIENTED_EDGE('',*,*,#5082,.T.);
#6343=ORIENTED_EDGE('',*,*,#5096,.F.);
#6344=ORIENTED_EDGE('',*,*,#5097,.F.);
#6345=ORIENTED_EDGE('',*,*,#5098,.T.);
#6346=ORIENTED_EDGE('',*,*,#5099,.F.);
#6347=ORIENTED_EDGE('',*,*,#5100,.F.);
#6348=ORIENTED_EDGE('',*,*,#5101,.F.);
#6349=ORIENTED_EDGE('',*,*,#5102,.T.);
#6350=ORIENTED_EDGE('',*,*,#5103,.F.);
#6351=ORIENTED_EDGE('',*,*,#5104,.F.);
#6352=ORIENTED_EDGE('',*,*,#5105,.T.);
#6353=ORIENTED_EDGE('',*,*,#5106,.F.);
#6354=ORIENTED_EDGE('',*,*,#5107,.F.);
#6355=ORIENTED_EDGE('',*,*,#5108,.F.);
#6356=ORIENTED_EDGE('',*,*,#5109,.F.);
#6357=ORIENTED_EDGE('',*,*,#5105,.F.);
#6358=ORIENTED_EDGE('',*,*,#5110,.F.);
#6359=ORIENTED_EDGE('',*,*,#5111,.T.);
#6360=ORIENTED_EDGE('',*,*,#5112,.F.);
#6361=ORIENTED_EDGE('',*,*,#5111,.F.);
#6362=ORIENTED_EDGE('',*,*,#5113,.F.);
#6363=ORIENTED_EDGE('',*,*,#5107,.T.);
#6364=ORIENTED_EDGE('',*,*,#5100,.T.);
#6365=ORIENTED_EDGE('',*,*,#5114,.F.);
#6366=ORIENTED_EDGE('',*,*,#5115,.F.);
#6367=ORIENTED_EDGE('',*,*,#5116,.F.);
#6368=ORIENTED_EDGE('',*,*,#5101,.T.);
#6369=ORIENTED_EDGE('',*,*,#5116,.T.);
#6370=ORIENTED_EDGE('',*,*,#5117,.F.);
#6371=ORIENTED_EDGE('',*,*,#5096,.T.);
#6372=ORIENTED_EDGE('',*,*,#5118,.F.);
#6373=ORIENTED_EDGE('',*,*,#5119,.F.);
#6374=ORIENTED_EDGE('',*,*,#5120,.F.);
#6375=ORIENTED_EDGE('',*,*,#5097,.T.);
#6376=ORIENTED_EDGE('',*,*,#5120,.T.);
#6377=ORIENTED_EDGE('',*,*,#5121,.F.);
#6378=ORIENTED_EDGE('',*,*,#5122,.T.);
#6379=ORIENTED_EDGE('',*,*,#5123,.T.);
#6380=ORIENTED_EDGE('',*,*,#5114,.T.);
#6381=ORIENTED_EDGE('',*,*,#5103,.T.);
#6382=ORIENTED_EDGE('',*,*,#5124,.T.);
#6383=ORIENTED_EDGE('',*,*,#5125,.T.);
#6384=ORIENTED_EDGE('',*,*,#5126,.T.);
#6385=ORIENTED_EDGE('',*,*,#5118,.T.);
#6386=ORIENTED_EDGE('',*,*,#5099,.T.);
#6387=ORIENTED_EDGE('',*,*,#5127,.T.);
#6388=ORIENTED_EDGE('',*,*,#5112,.T.);
#6389=ORIENTED_EDGE('',*,*,#5128,.F.);
#6390=ORIENTED_EDGE('',*,*,#5129,.T.);
#6391=ORIENTED_EDGE('',*,*,#5117,.T.);
#6392=ORIENTED_EDGE('',*,*,#5129,.F.);
#6393=ORIENTED_EDGE('',*,*,#5130,.F.);
#6394=ORIENTED_EDGE('',*,*,#5131,.T.);
#6395=ORIENTED_EDGE('',*,*,#5121,.T.);
#6396=ORIENTED_EDGE('',*,*,#5131,.F.);
#6397=ORIENTED_EDGE('',*,*,#5132,.F.);
#6398=ORIENTED_EDGE('',*,*,#5133,.T.);
#6399=ORIENTED_EDGE('',*,*,#5110,.T.);
#6400=ORIENTED_EDGE('',*,*,#5104,.T.);
#6401=ORIENTED_EDGE('',*,*,#5109,.T.);
#6402=ORIENTED_EDGE('',*,*,#5134,.T.);
#6403=ORIENTED_EDGE('',*,*,#5135,.F.);
#6404=ORIENTED_EDGE('',*,*,#5134,.F.);
#6405=ORIENTED_EDGE('',*,*,#5108,.T.);
#6406=ORIENTED_EDGE('',*,*,#5113,.T.);
#6407=ORIENTED_EDGE('',*,*,#5106,.T.);
#6408=ORIENTED_EDGE('',*,*,#5133,.F.);
#6409=ORIENTED_EDGE('',*,*,#5136,.T.);
#6410=ORIENTED_EDGE('',*,*,#5137,.T.);
#6411=ORIENTED_EDGE('',*,*,#5127,.F.);
#6412=ORIENTED_EDGE('',*,*,#5098,.F.);
#6413=ORIENTED_EDGE('',*,*,#5119,.T.);
#6414=ORIENTED_EDGE('',*,*,#5126,.F.);
#6415=ORIENTED_EDGE('',*,*,#5138,.F.);
#6416=ORIENTED_EDGE('',*,*,#5139,.T.);
#6417=ORIENTED_EDGE('',*,*,#5138,.T.);
#6418=ORIENTED_EDGE('',*,*,#5125,.F.);
#6419=ORIENTED_EDGE('',*,*,#5140,.F.);
#6420=ORIENTED_EDGE('',*,*,#5135,.T.);
#6421=ORIENTED_EDGE('',*,*,#5141,.T.);
#6422=ORIENTED_EDGE('',*,*,#5140,.T.);
#6423=ORIENTED_EDGE('',*,*,#5124,.F.);
#6424=ORIENTED_EDGE('',*,*,#5102,.F.);
#6425=ORIENTED_EDGE('',*,*,#5115,.T.);
#6426=ORIENTED_EDGE('',*,*,#5123,.F.);
#6427=ORIENTED_EDGE('',*,*,#5142,.F.);
#6428=ORIENTED_EDGE('',*,*,#5143,.T.);
#6429=ORIENTED_EDGE('',*,*,#5142,.T.);
#6430=ORIENTED_EDGE('',*,*,#5122,.F.);
#6431=ORIENTED_EDGE('',*,*,#5137,.F.);
#6432=ORIENTED_EDGE('',*,*,#5132,.T.);
#6433=ORIENTED_EDGE('',*,*,#5143,.F.);
#6434=ORIENTED_EDGE('',*,*,#5136,.F.);
#6435=ORIENTED_EDGE('',*,*,#5139,.F.);
#6436=ORIENTED_EDGE('',*,*,#5141,.F.);
#6437=ORIENTED_EDGE('',*,*,#5128,.T.);
#6438=ORIENTED_EDGE('',*,*,#5130,.T.);
#6439=ORIENTED_EDGE('',*,*,#5144,.F.);
#6440=ORIENTED_EDGE('',*,*,#5145,.F.);
#6441=ORIENTED_EDGE('',*,*,#5146,.T.);
#6442=ORIENTED_EDGE('',*,*,#5147,.F.);
#6443=ORIENTED_EDGE('',*,*,#5148,.F.);
#6444=ORIENTED_EDGE('',*,*,#5149,.F.);
#6445=ORIENTED_EDGE('',*,*,#5150,.T.);
#6446=ORIENTED_EDGE('',*,*,#5151,.F.);
#6447=ORIENTED_EDGE('',*,*,#5152,.F.);
#6448=ORIENTED_EDGE('',*,*,#5153,.T.);
#6449=ORIENTED_EDGE('',*,*,#5154,.F.);
#6450=ORIENTED_EDGE('',*,*,#5155,.F.);
#6451=ORIENTED_EDGE('',*,*,#5156,.F.);
#6452=ORIENTED_EDGE('',*,*,#5157,.F.);
#6453=ORIENTED_EDGE('',*,*,#5153,.F.);
#6454=ORIENTED_EDGE('',*,*,#5158,.F.);
#6455=ORIENTED_EDGE('',*,*,#5159,.T.);
#6456=ORIENTED_EDGE('',*,*,#5160,.F.);
#6457=ORIENTED_EDGE('',*,*,#5159,.F.);
#6458=ORIENTED_EDGE('',*,*,#5161,.F.);
#6459=ORIENTED_EDGE('',*,*,#5155,.T.);
#6460=ORIENTED_EDGE('',*,*,#5148,.T.);
#6461=ORIENTED_EDGE('',*,*,#5162,.F.);
#6462=ORIENTED_EDGE('',*,*,#5163,.F.);
#6463=ORIENTED_EDGE('',*,*,#5164,.F.);
#6464=ORIENTED_EDGE('',*,*,#5149,.T.);
#6465=ORIENTED_EDGE('',*,*,#5164,.T.);
#6466=ORIENTED_EDGE('',*,*,#5165,.F.);
#6467=ORIENTED_EDGE('',*,*,#5144,.T.);
#6468=ORIENTED_EDGE('',*,*,#5166,.F.);
#6469=ORIENTED_EDGE('',*,*,#5167,.F.);
#6470=ORIENTED_EDGE('',*,*,#5168,.F.);
#6471=ORIENTED_EDGE('',*,*,#5145,.T.);
#6472=ORIENTED_EDGE('',*,*,#5168,.T.);
#6473=ORIENTED_EDGE('',*,*,#5169,.F.);
#6474=ORIENTED_EDGE('',*,*,#5170,.T.);
#6475=ORIENTED_EDGE('',*,*,#5171,.T.);
#6476=ORIENTED_EDGE('',*,*,#5162,.T.);
#6477=ORIENTED_EDGE('',*,*,#5151,.T.);
#6478=ORIENTED_EDGE('',*,*,#5172,.T.);
#6479=ORIENTED_EDGE('',*,*,#5173,.T.);
#6480=ORIENTED_EDGE('',*,*,#5174,.T.);
#6481=ORIENTED_EDGE('',*,*,#5166,.T.);
#6482=ORIENTED_EDGE('',*,*,#5147,.T.);
#6483=ORIENTED_EDGE('',*,*,#5175,.T.);
#6484=ORIENTED_EDGE('',*,*,#5160,.T.);
#6485=ORIENTED_EDGE('',*,*,#5176,.F.);
#6486=ORIENTED_EDGE('',*,*,#5177,.T.);
#6487=ORIENTED_EDGE('',*,*,#5165,.T.);
#6488=ORIENTED_EDGE('',*,*,#5177,.F.);
#6489=ORIENTED_EDGE('',*,*,#5178,.F.);
#6490=ORIENTED_EDGE('',*,*,#5179,.T.);
#6491=ORIENTED_EDGE('',*,*,#5169,.T.);
#6492=ORIENTED_EDGE('',*,*,#5179,.F.);
#6493=ORIENTED_EDGE('',*,*,#5180,.F.);
#6494=ORIENTED_EDGE('',*,*,#5181,.T.);
#6495=ORIENTED_EDGE('',*,*,#5158,.T.);
#6496=ORIENTED_EDGE('',*,*,#5152,.T.);
#6497=ORIENTED_EDGE('',*,*,#5157,.T.);
#6498=ORIENTED_EDGE('',*,*,#5182,.T.);
#6499=ORIENTED_EDGE('',*,*,#5183,.F.);
#6500=ORIENTED_EDGE('',*,*,#5182,.F.);
#6501=ORIENTED_EDGE('',*,*,#5156,.T.);
#6502=ORIENTED_EDGE('',*,*,#5161,.T.);
#6503=ORIENTED_EDGE('',*,*,#5154,.T.);
#6504=ORIENTED_EDGE('',*,*,#5181,.F.);
#6505=ORIENTED_EDGE('',*,*,#5184,.T.);
#6506=ORIENTED_EDGE('',*,*,#5185,.T.);
#6507=ORIENTED_EDGE('',*,*,#5175,.F.);
#6508=ORIENTED_EDGE('',*,*,#5146,.F.);
#6509=ORIENTED_EDGE('',*,*,#5167,.T.);
#6510=ORIENTED_EDGE('',*,*,#5174,.F.);
#6511=ORIENTED_EDGE('',*,*,#5186,.F.);
#6512=ORIENTED_EDGE('',*,*,#5187,.T.);
#6513=ORIENTED_EDGE('',*,*,#5186,.T.);
#6514=ORIENTED_EDGE('',*,*,#5173,.F.);
#6515=ORIENTED_EDGE('',*,*,#5188,.F.);
#6516=ORIENTED_EDGE('',*,*,#5183,.T.);
#6517=ORIENTED_EDGE('',*,*,#5189,.T.);
#6518=ORIENTED_EDGE('',*,*,#5188,.T.);
#6519=ORIENTED_EDGE('',*,*,#5172,.F.);
#6520=ORIENTED_EDGE('',*,*,#5150,.F.);
#6521=ORIENTED_EDGE('',*,*,#5163,.T.);
#6522=ORIENTED_EDGE('',*,*,#5171,.F.);
#6523=ORIENTED_EDGE('',*,*,#5190,.F.);
#6524=ORIENTED_EDGE('',*,*,#5191,.T.);
#6525=ORIENTED_EDGE('',*,*,#5190,.T.);
#6526=ORIENTED_EDGE('',*,*,#5170,.F.);
#6527=ORIENTED_EDGE('',*,*,#5185,.F.);
#6528=ORIENTED_EDGE('',*,*,#5180,.T.);
#6529=ORIENTED_EDGE('',*,*,#5191,.F.);
#6530=ORIENTED_EDGE('',*,*,#5184,.F.);
#6531=ORIENTED_EDGE('',*,*,#5187,.F.);
#6532=ORIENTED_EDGE('',*,*,#5189,.F.);
#6533=ORIENTED_EDGE('',*,*,#5176,.T.);
#6534=ORIENTED_EDGE('',*,*,#5178,.T.);
#6535=ORIENTED_EDGE('',*,*,#5192,.F.);
#6536=ORIENTED_EDGE('',*,*,#5193,.F.);
#6537=ORIENTED_EDGE('',*,*,#5194,.T.);
#6538=ORIENTED_EDGE('',*,*,#5195,.F.);
#6539=ORIENTED_EDGE('',*,*,#5196,.F.);
#6540=ORIENTED_EDGE('',*,*,#5197,.F.);
#6541=ORIENTED_EDGE('',*,*,#5198,.T.);
#6542=ORIENTED_EDGE('',*,*,#5199,.F.);
#6543=ORIENTED_EDGE('',*,*,#5200,.F.);
#6544=ORIENTED_EDGE('',*,*,#5201,.T.);
#6545=ORIENTED_EDGE('',*,*,#5202,.F.);
#6546=ORIENTED_EDGE('',*,*,#5203,.F.);
#6547=ORIENTED_EDGE('',*,*,#5204,.F.);
#6548=ORIENTED_EDGE('',*,*,#5205,.F.);
#6549=ORIENTED_EDGE('',*,*,#5201,.F.);
#6550=ORIENTED_EDGE('',*,*,#5206,.F.);
#6551=ORIENTED_EDGE('',*,*,#5207,.T.);
#6552=ORIENTED_EDGE('',*,*,#5208,.F.);
#6553=ORIENTED_EDGE('',*,*,#5207,.F.);
#6554=ORIENTED_EDGE('',*,*,#5209,.F.);
#6555=ORIENTED_EDGE('',*,*,#5203,.T.);
#6556=ORIENTED_EDGE('',*,*,#5196,.T.);
#6557=ORIENTED_EDGE('',*,*,#5210,.F.);
#6558=ORIENTED_EDGE('',*,*,#5211,.F.);
#6559=ORIENTED_EDGE('',*,*,#5212,.F.);
#6560=ORIENTED_EDGE('',*,*,#5197,.T.);
#6561=ORIENTED_EDGE('',*,*,#5212,.T.);
#6562=ORIENTED_EDGE('',*,*,#5213,.F.);
#6563=ORIENTED_EDGE('',*,*,#5192,.T.);
#6564=ORIENTED_EDGE('',*,*,#5214,.F.);
#6565=ORIENTED_EDGE('',*,*,#5215,.F.);
#6566=ORIENTED_EDGE('',*,*,#5216,.F.);
#6567=ORIENTED_EDGE('',*,*,#5193,.T.);
#6568=ORIENTED_EDGE('',*,*,#5216,.T.);
#6569=ORIENTED_EDGE('',*,*,#5217,.F.);
#6570=ORIENTED_EDGE('',*,*,#5218,.T.);
#6571=ORIENTED_EDGE('',*,*,#5219,.T.);
#6572=ORIENTED_EDGE('',*,*,#5210,.T.);
#6573=ORIENTED_EDGE('',*,*,#5199,.T.);
#6574=ORIENTED_EDGE('',*,*,#5220,.T.);
#6575=ORIENTED_EDGE('',*,*,#5221,.T.);
#6576=ORIENTED_EDGE('',*,*,#5222,.T.);
#6577=ORIENTED_EDGE('',*,*,#5214,.T.);
#6578=ORIENTED_EDGE('',*,*,#5195,.T.);
#6579=ORIENTED_EDGE('',*,*,#5223,.T.);
#6580=ORIENTED_EDGE('',*,*,#5208,.T.);
#6581=ORIENTED_EDGE('',*,*,#5224,.F.);
#6582=ORIENTED_EDGE('',*,*,#5225,.T.);
#6583=ORIENTED_EDGE('',*,*,#5213,.T.);
#6584=ORIENTED_EDGE('',*,*,#5225,.F.);
#6585=ORIENTED_EDGE('',*,*,#5226,.F.);
#6586=ORIENTED_EDGE('',*,*,#5227,.T.);
#6587=ORIENTED_EDGE('',*,*,#5217,.T.);
#6588=ORIENTED_EDGE('',*,*,#5227,.F.);
#6589=ORIENTED_EDGE('',*,*,#5228,.F.);
#6590=ORIENTED_EDGE('',*,*,#5229,.T.);
#6591=ORIENTED_EDGE('',*,*,#5206,.T.);
#6592=ORIENTED_EDGE('',*,*,#5200,.T.);
#6593=ORIENTED_EDGE('',*,*,#5205,.T.);
#6594=ORIENTED_EDGE('',*,*,#5230,.T.);
#6595=ORIENTED_EDGE('',*,*,#5231,.F.);
#6596=ORIENTED_EDGE('',*,*,#5230,.F.);
#6597=ORIENTED_EDGE('',*,*,#5204,.T.);
#6598=ORIENTED_EDGE('',*,*,#5209,.T.);
#6599=ORIENTED_EDGE('',*,*,#5202,.T.);
#6600=ORIENTED_EDGE('',*,*,#5229,.F.);
#6601=ORIENTED_EDGE('',*,*,#5232,.T.);
#6602=ORIENTED_EDGE('',*,*,#5233,.T.);
#6603=ORIENTED_EDGE('',*,*,#5223,.F.);
#6604=ORIENTED_EDGE('',*,*,#5194,.F.);
#6605=ORIENTED_EDGE('',*,*,#5215,.T.);
#6606=ORIENTED_EDGE('',*,*,#5222,.F.);
#6607=ORIENTED_EDGE('',*,*,#5234,.F.);
#6608=ORIENTED_EDGE('',*,*,#5235,.T.);
#6609=ORIENTED_EDGE('',*,*,#5234,.T.);
#6610=ORIENTED_EDGE('',*,*,#5221,.F.);
#6611=ORIENTED_EDGE('',*,*,#5236,.F.);
#6612=ORIENTED_EDGE('',*,*,#5231,.T.);
#6613=ORIENTED_EDGE('',*,*,#5237,.T.);
#6614=ORIENTED_EDGE('',*,*,#5236,.T.);
#6615=ORIENTED_EDGE('',*,*,#5220,.F.);
#6616=ORIENTED_EDGE('',*,*,#5198,.F.);
#6617=ORIENTED_EDGE('',*,*,#5211,.T.);
#6618=ORIENTED_EDGE('',*,*,#5219,.F.);
#6619=ORIENTED_EDGE('',*,*,#5238,.F.);
#6620=ORIENTED_EDGE('',*,*,#5239,.T.);
#6621=ORIENTED_EDGE('',*,*,#5238,.T.);
#6622=ORIENTED_EDGE('',*,*,#5218,.F.);
#6623=ORIENTED_EDGE('',*,*,#5233,.F.);
#6624=ORIENTED_EDGE('',*,*,#5228,.T.);
#6625=ORIENTED_EDGE('',*,*,#5239,.F.);
#6626=ORIENTED_EDGE('',*,*,#5232,.F.);
#6627=ORIENTED_EDGE('',*,*,#5235,.F.);
#6628=ORIENTED_EDGE('',*,*,#5237,.F.);
#6629=ORIENTED_EDGE('',*,*,#5224,.T.);
#6630=ORIENTED_EDGE('',*,*,#5226,.T.);
#6631=ORIENTED_EDGE('',*,*,#5240,.F.);
#6632=ORIENTED_EDGE('',*,*,#5241,.T.);
#6633=ORIENTED_EDGE('',*,*,#5242,.F.);
#6634=ORIENTED_EDGE('',*,*,#5241,.F.);
#6635=ORIENTED_EDGE('',*,*,#5243,.F.);
#6636=ORIENTED_EDGE('',*,*,#5244,.T.);
#6637=ORIENTED_EDGE('',*,*,#5245,.F.);
#6638=ORIENTED_EDGE('',*,*,#5244,.F.);
#6639=ORIENTED_EDGE('',*,*,#5246,.F.);
#6640=ORIENTED_EDGE('',*,*,#5247,.T.);
#6641=ORIENTED_EDGE('',*,*,#5248,.F.);
#6642=ORIENTED_EDGE('',*,*,#5247,.F.);
#6643=ORIENTED_EDGE('',*,*,#5249,.F.);
#6644=ORIENTED_EDGE('',*,*,#5250,.T.);
#6645=ORIENTED_EDGE('',*,*,#5251,.F.);
#6646=ORIENTED_EDGE('',*,*,#5250,.F.);
#6647=ORIENTED_EDGE('',*,*,#5252,.F.);
#6648=ORIENTED_EDGE('',*,*,#5253,.T.);
#6649=ORIENTED_EDGE('',*,*,#5254,.F.);
#6650=ORIENTED_EDGE('',*,*,#5253,.F.);
#6651=ORIENTED_EDGE('',*,*,#5255,.F.);
#6652=ORIENTED_EDGE('',*,*,#5256,.T.);
#6653=ORIENTED_EDGE('',*,*,#5257,.F.);
#6654=ORIENTED_EDGE('',*,*,#5256,.F.);
#6655=ORIENTED_EDGE('',*,*,#5258,.F.);
#6656=ORIENTED_EDGE('',*,*,#5259,.T.);
#6657=ORIENTED_EDGE('',*,*,#5260,.F.);
#6658=ORIENTED_EDGE('',*,*,#5259,.F.);
#6659=ORIENTED_EDGE('',*,*,#5261,.F.);
#6660=ORIENTED_EDGE('',*,*,#5262,.F.);
#6661=ORIENTED_EDGE('',*,*,#5263,.F.);
#6662=ORIENTED_EDGE('',*,*,#5264,.T.);
#6663=ORIENTED_EDGE('',*,*,#5257,.T.);
#6664=ORIENTED_EDGE('',*,*,#5265,.F.);
#6665=ORIENTED_EDGE('',*,*,#5266,.T.);
#6666=ORIENTED_EDGE('',*,*,#5267,.T.);
#6667=ORIENTED_EDGE('',*,*,#5268,.F.);
#6668=ORIENTED_EDGE('',*,*,#5254,.T.);
#6669=ORIENTED_EDGE('',*,*,#5269,.T.);
#6670=ORIENTED_EDGE('',*,*,#5263,.T.);
#6671=ORIENTED_EDGE('',*,*,#5270,.F.);
#6672=ORIENTED_EDGE('',*,*,#5271,.F.);
#6673=ORIENTED_EDGE('',*,*,#5272,.T.);
#6674=ORIENTED_EDGE('',*,*,#5273,.T.);
#6675=ORIENTED_EDGE('',*,*,#5274,.F.);
#6676=ORIENTED_EDGE('',*,*,#5267,.F.);
#6677=ORIENTED_EDGE('',*,*,#5265,.T.);
#6678=ORIENTED_EDGE('',*,*,#5275,.T.);
#6679=ORIENTED_EDGE('',*,*,#5276,.F.);
#6680=ORIENTED_EDGE('',*,*,#5277,.F.);
#6681=ORIENTED_EDGE('',*,*,#5278,.T.);
#6682=ORIENTED_EDGE('',*,*,#5279,.F.);
#6683=ORIENTED_EDGE('',*,*,#5275,.F.);
#6684=ORIENTED_EDGE('',*,*,#5268,.T.);
#6685=ORIENTED_EDGE('',*,*,#5274,.T.);
#6686=ORIENTED_EDGE('',*,*,#5280,.T.);
#6687=ORIENTED_EDGE('',*,*,#5270,.T.);
#6688=ORIENTED_EDGE('',*,*,#5262,.T.);
#6689=ORIENTED_EDGE('',*,*,#5260,.T.);
#6690=ORIENTED_EDGE('',*,*,#5251,.T.);
#6691=ORIENTED_EDGE('',*,*,#5248,.T.);
#6692=ORIENTED_EDGE('',*,*,#5245,.T.);
#6693=ORIENTED_EDGE('',*,*,#5242,.T.);
#6694=ORIENTED_EDGE('',*,*,#5261,.T.);
#6695=ORIENTED_EDGE('',*,*,#5281,.T.);
#6696=ORIENTED_EDGE('',*,*,#5282,.F.);
#6697=ORIENTED_EDGE('',*,*,#5278,.F.);
#6698=ORIENTED_EDGE('',*,*,#5277,.T.);
#6699=ORIENTED_EDGE('',*,*,#5283,.F.);
#6700=ORIENTED_EDGE('',*,*,#5281,.F.);
#6701=ORIENTED_EDGE('',*,*,#5264,.F.);
#6702=ORIENTED_EDGE('',*,*,#5269,.F.);
#6703=ORIENTED_EDGE('',*,*,#5284,.T.);
#6704=ORIENTED_EDGE('',*,*,#5272,.F.);
#6705=ORIENTED_EDGE('',*,*,#5266,.F.);
#6706=ORIENTED_EDGE('',*,*,#5258,.T.);
#6707=ORIENTED_EDGE('',*,*,#5249,.T.);
#6708=ORIENTED_EDGE('',*,*,#5246,.T.);
#6709=ORIENTED_EDGE('',*,*,#5243,.T.);
#6710=ORIENTED_EDGE('',*,*,#5240,.T.);
#6711=ORIENTED_EDGE('',*,*,#5283,.T.);
#6712=ORIENTED_EDGE('',*,*,#5276,.T.);
#6713=ORIENTED_EDGE('',*,*,#5279,.T.);
#6714=ORIENTED_EDGE('',*,*,#5282,.T.);
#6715=ORIENTED_EDGE('',*,*,#5284,.F.);
#6716=ORIENTED_EDGE('',*,*,#5271,.T.);
#6717=ORIENTED_EDGE('',*,*,#5280,.F.);
#6718=ORIENTED_EDGE('',*,*,#5273,.F.);
#6719=ORIENTED_EDGE('',*,*,#5252,.T.);
#6720=ORIENTED_EDGE('',*,*,#5255,.T.);
#6721=ORIENTED_EDGE('',*,*,#5285,.F.);
#6722=ORIENTED_EDGE('',*,*,#5286,.T.);
#6723=ORIENTED_EDGE('',*,*,#5287,.F.);
#6724=ORIENTED_EDGE('',*,*,#5286,.F.);
#6725=ORIENTED_EDGE('',*,*,#5288,.F.);
#6726=ORIENTED_EDGE('',*,*,#5289,.T.);
#6727=ORIENTED_EDGE('',*,*,#5290,.F.);
#6728=ORIENTED_EDGE('',*,*,#5289,.F.);
#6729=ORIENTED_EDGE('',*,*,#5291,.F.);
#6730=ORIENTED_EDGE('',*,*,#5292,.T.);
#6731=ORIENTED_EDGE('',*,*,#5293,.F.);
#6732=ORIENTED_EDGE('',*,*,#5292,.F.);
#6733=ORIENTED_EDGE('',*,*,#5294,.F.);
#6734=ORIENTED_EDGE('',*,*,#5295,.T.);
#6735=ORIENTED_EDGE('',*,*,#5296,.F.);
#6736=ORIENTED_EDGE('',*,*,#5295,.F.);
#6737=ORIENTED_EDGE('',*,*,#5297,.F.);
#6738=ORIENTED_EDGE('',*,*,#5298,.T.);
#6739=ORIENTED_EDGE('',*,*,#5299,.F.);
#6740=ORIENTED_EDGE('',*,*,#5298,.F.);
#6741=ORIENTED_EDGE('',*,*,#5297,.T.);
#6742=ORIENTED_EDGE('',*,*,#5300,.T.);
#6743=ORIENTED_EDGE('',*,*,#5300,.F.);
#6744=ORIENTED_EDGE('',*,*,#5301,.T.);
#6745=ORIENTED_EDGE('',*,*,#5302,.T.);
#6746=ORIENTED_EDGE('',*,*,#5301,.F.);
#6747=ORIENTED_EDGE('',*,*,#5303,.F.);
#6748=ORIENTED_EDGE('',*,*,#5304,.T.);
#6749=ORIENTED_EDGE('',*,*,#5305,.T.);
#6750=ORIENTED_EDGE('',*,*,#5304,.F.);
#6751=ORIENTED_EDGE('',*,*,#5303,.T.);
#6752=ORIENTED_EDGE('',*,*,#5299,.T.);
#6753=ORIENTED_EDGE('',*,*,#5296,.T.);
#6754=ORIENTED_EDGE('',*,*,#5293,.T.);
#6755=ORIENTED_EDGE('',*,*,#5290,.T.);
#6756=ORIENTED_EDGE('',*,*,#5287,.T.);
#6757=ORIENTED_EDGE('',*,*,#5305,.F.);
#6758=ORIENTED_EDGE('',*,*,#5302,.F.);
#6759=ORIENTED_EDGE('',*,*,#5294,.T.);
#6760=ORIENTED_EDGE('',*,*,#5291,.T.);
#6761=ORIENTED_EDGE('',*,*,#5288,.T.);
#6762=ORIENTED_EDGE('',*,*,#5285,.T.);
#6763=ORIENTED_EDGE('',*,*,#5306,.F.);
#6764=ORIENTED_EDGE('',*,*,#5307,.T.);
#6765=ORIENTED_EDGE('',*,*,#5308,.F.);
#6766=ORIENTED_EDGE('',*,*,#5307,.F.);
#6767=ORIENTED_EDGE('',*,*,#5309,.F.);
#6768=ORIENTED_EDGE('',*,*,#5310,.T.);
#6769=ORIENTED_EDGE('',*,*,#5311,.F.);
#6770=ORIENTED_EDGE('',*,*,#5310,.F.);
#6771=ORIENTED_EDGE('',*,*,#5312,.F.);
#6772=ORIENTED_EDGE('',*,*,#5313,.T.);
#6773=ORIENTED_EDGE('',*,*,#5314,.F.);
#6774=ORIENTED_EDGE('',*,*,#5313,.F.);
#6775=ORIENTED_EDGE('',*,*,#5315,.F.);
#6776=ORIENTED_EDGE('',*,*,#5316,.T.);
#6777=ORIENTED_EDGE('',*,*,#5317,.F.);
#6778=ORIENTED_EDGE('',*,*,#5316,.F.);
#6779=ORIENTED_EDGE('',*,*,#5318,.F.);
#6780=ORIENTED_EDGE('',*,*,#5319,.T.);
#6781=ORIENTED_EDGE('',*,*,#5320,.T.);
#6782=ORIENTED_EDGE('',*,*,#5319,.F.);
#6783=ORIENTED_EDGE('',*,*,#5320,.F.);
#6784=ORIENTED_EDGE('',*,*,#5321,.F.);
#6785=ORIENTED_EDGE('',*,*,#5322,.F.);
#6786=ORIENTED_EDGE('',*,*,#5323,.T.);
#6787=ORIENTED_EDGE('',*,*,#5321,.T.);
#6788=ORIENTED_EDGE('',*,*,#5323,.F.);
#6789=ORIENTED_EDGE('',*,*,#5324,.F.);
#6790=ORIENTED_EDGE('',*,*,#5325,.T.);
#6791=ORIENTED_EDGE('',*,*,#5326,.T.);
#6792=ORIENTED_EDGE('',*,*,#5325,.F.);
#6793=ORIENTED_EDGE('',*,*,#5324,.T.);
#6794=ORIENTED_EDGE('',*,*,#5322,.T.);
#6795=ORIENTED_EDGE('',*,*,#5317,.T.);
#6796=ORIENTED_EDGE('',*,*,#5314,.T.);
#6797=ORIENTED_EDGE('',*,*,#5311,.T.);
#6798=ORIENTED_EDGE('',*,*,#5308,.T.);
#6799=ORIENTED_EDGE('',*,*,#5326,.F.);
#6800=ORIENTED_EDGE('',*,*,#5318,.T.);
#6801=ORIENTED_EDGE('',*,*,#5315,.T.);
#6802=ORIENTED_EDGE('',*,*,#5312,.T.);
#6803=ORIENTED_EDGE('',*,*,#5309,.T.);
#6804=ORIENTED_EDGE('',*,*,#5306,.T.);
#6805=ORIENTED_EDGE('',*,*,#5327,.F.);
#6806=ORIENTED_EDGE('',*,*,#5328,.T.);
#6807=ORIENTED_EDGE('',*,*,#5329,.F.);
#6808=ORIENTED_EDGE('',*,*,#5328,.F.);
#6809=ORIENTED_EDGE('',*,*,#5330,.F.);
#6810=ORIENTED_EDGE('',*,*,#5331,.T.);
#6811=ORIENTED_EDGE('',*,*,#5332,.F.);
#6812=ORIENTED_EDGE('',*,*,#5331,.F.);
#6813=ORIENTED_EDGE('',*,*,#5333,.F.);
#6814=ORIENTED_EDGE('',*,*,#5334,.T.);
#6815=ORIENTED_EDGE('',*,*,#5335,.F.);
#6816=ORIENTED_EDGE('',*,*,#5334,.F.);
#6817=ORIENTED_EDGE('',*,*,#5336,.F.);
#6818=ORIENTED_EDGE('',*,*,#5337,.T.);
#6819=ORIENTED_EDGE('',*,*,#5338,.F.);
#6820=ORIENTED_EDGE('',*,*,#5337,.F.);
#6821=ORIENTED_EDGE('',*,*,#5339,.F.);
#6822=ORIENTED_EDGE('',*,*,#5340,.T.);
#6823=ORIENTED_EDGE('',*,*,#5341,.F.);
#6824=ORIENTED_EDGE('',*,*,#5340,.F.);
#6825=ORIENTED_EDGE('',*,*,#5342,.F.);
#6826=ORIENTED_EDGE('',*,*,#5343,.T.);
#6827=ORIENTED_EDGE('',*,*,#5344,.F.);
#6828=ORIENTED_EDGE('',*,*,#5343,.F.);
#6829=ORIENTED_EDGE('',*,*,#5345,.F.);
#6830=ORIENTED_EDGE('',*,*,#5346,.T.);
#6831=ORIENTED_EDGE('',*,*,#5347,.F.);
#6832=ORIENTED_EDGE('',*,*,#5346,.F.);
#6833=ORIENTED_EDGE('',*,*,#5348,.F.);
#6834=ORIENTED_EDGE('',*,*,#5349,.F.);
#6835=ORIENTED_EDGE('',*,*,#5350,.F.);
#6836=ORIENTED_EDGE('',*,*,#5351,.T.);
#6837=ORIENTED_EDGE('',*,*,#5344,.T.);
#6838=ORIENTED_EDGE('',*,*,#5352,.F.);
#6839=ORIENTED_EDGE('',*,*,#5353,.T.);
#6840=ORIENTED_EDGE('',*,*,#5354,.T.);
#6841=ORIENTED_EDGE('',*,*,#5355,.F.);
#6842=ORIENTED_EDGE('',*,*,#5341,.T.);
#6843=ORIENTED_EDGE('',*,*,#5356,.T.);
#6844=ORIENTED_EDGE('',*,*,#5350,.T.);
#6845=ORIENTED_EDGE('',*,*,#5357,.F.);
#6846=ORIENTED_EDGE('',*,*,#5358,.F.);
#6847=ORIENTED_EDGE('',*,*,#5359,.T.);
#6848=ORIENTED_EDGE('',*,*,#5360,.T.);
#6849=ORIENTED_EDGE('',*,*,#5361,.F.);
#6850=ORIENTED_EDGE('',*,*,#5354,.F.);
#6851=ORIENTED_EDGE('',*,*,#5352,.T.);
#6852=ORIENTED_EDGE('',*,*,#5362,.T.);
#6853=ORIENTED_EDGE('',*,*,#5363,.F.);
#6854=ORIENTED_EDGE('',*,*,#5364,.F.);
#6855=ORIENTED_EDGE('',*,*,#5365,.T.);
#6856=ORIENTED_EDGE('',*,*,#5366,.F.);
#6857=ORIENTED_EDGE('',*,*,#5362,.F.);
#6858=ORIENTED_EDGE('',*,*,#5355,.T.);
#6859=ORIENTED_EDGE('',*,*,#5361,.T.);
#6860=ORIENTED_EDGE('',*,*,#5367,.T.);
#6861=ORIENTED_EDGE('',*,*,#5357,.T.);
#6862=ORIENTED_EDGE('',*,*,#5349,.T.);
#6863=ORIENTED_EDGE('',*,*,#5347,.T.);
#6864=ORIENTED_EDGE('',*,*,#5338,.T.);
#6865=ORIENTED_EDGE('',*,*,#5335,.T.);
#6866=ORIENTED_EDGE('',*,*,#5332,.T.);
#6867=ORIENTED_EDGE('',*,*,#5329,.T.);
#6868=ORIENTED_EDGE('',*,*,#5348,.T.);
#6869=ORIENTED_EDGE('',*,*,#5368,.T.);
#6870=ORIENTED_EDGE('',*,*,#5369,.F.);
#6871=ORIENTED_EDGE('',*,*,#5365,.F.);
#6872=ORIENTED_EDGE('',*,*,#5364,.T.);
#6873=ORIENTED_EDGE('',*,*,#5370,.F.);
#6874=ORIENTED_EDGE('',*,*,#5368,.F.);
#6875=ORIENTED_EDGE('',*,*,#5351,.F.);
#6876=ORIENTED_EDGE('',*,*,#5356,.F.);
#6877=ORIENTED_EDGE('',*,*,#5371,.T.);
#6878=ORIENTED_EDGE('',*,*,#5359,.F.);
#6879=ORIENTED_EDGE('',*,*,#5353,.F.);
#6880=ORIENTED_EDGE('',*,*,#5345,.T.);
#6881=ORIENTED_EDGE('',*,*,#5336,.T.);
#6882=ORIENTED_EDGE('',*,*,#5333,.T.);
#6883=ORIENTED_EDGE('',*,*,#5330,.T.);
#6884=ORIENTED_EDGE('',*,*,#5327,.T.);
#6885=ORIENTED_EDGE('',*,*,#5370,.T.);
#6886=ORIENTED_EDGE('',*,*,#5363,.T.);
#6887=ORIENTED_EDGE('',*,*,#5366,.T.);
#6888=ORIENTED_EDGE('',*,*,#5369,.T.);
#6889=ORIENTED_EDGE('',*,*,#5371,.F.);
#6890=ORIENTED_EDGE('',*,*,#5358,.T.);
#6891=ORIENTED_EDGE('',*,*,#5367,.F.);
#6892=ORIENTED_EDGE('',*,*,#5360,.F.);
#6893=ORIENTED_EDGE('',*,*,#5339,.T.);
#6894=ORIENTED_EDGE('',*,*,#5342,.T.);
#6895=ORIENTED_EDGE('',*,*,#5372,.F.);
#6896=ORIENTED_EDGE('',*,*,#5373,.T.);
#6897=ORIENTED_EDGE('',*,*,#5374,.F.);
#6898=ORIENTED_EDGE('',*,*,#5373,.F.);
#6899=ORIENTED_EDGE('',*,*,#5375,.F.);
#6900=ORIENTED_EDGE('',*,*,#5376,.T.);
#6901=ORIENTED_EDGE('',*,*,#5377,.F.);
#6902=ORIENTED_EDGE('',*,*,#5376,.F.);
#6903=ORIENTED_EDGE('',*,*,#5378,.F.);
#6904=ORIENTED_EDGE('',*,*,#5379,.T.);
#6905=ORIENTED_EDGE('',*,*,#5380,.F.);
#6906=ORIENTED_EDGE('',*,*,#5379,.F.);
#6907=ORIENTED_EDGE('',*,*,#5381,.F.);
#6908=ORIENTED_EDGE('',*,*,#5382,.T.);
#6909=ORIENTED_EDGE('',*,*,#5383,.F.);
#6910=ORIENTED_EDGE('',*,*,#5382,.F.);
#6911=ORIENTED_EDGE('',*,*,#5384,.F.);
#6912=ORIENTED_EDGE('',*,*,#5385,.T.);
#6913=ORIENTED_EDGE('',*,*,#5386,.F.);
#6914=ORIENTED_EDGE('',*,*,#5385,.F.);
#6915=ORIENTED_EDGE('',*,*,#5384,.T.);
#6916=ORIENTED_EDGE('',*,*,#5387,.T.);
#6917=ORIENTED_EDGE('',*,*,#5387,.F.);
#6918=ORIENTED_EDGE('',*,*,#5388,.T.);
#6919=ORIENTED_EDGE('',*,*,#5389,.T.);
#6920=ORIENTED_EDGE('',*,*,#5388,.F.);
#6921=ORIENTED_EDGE('',*,*,#5390,.F.);
#6922=ORIENTED_EDGE('',*,*,#5391,.T.);
#6923=ORIENTED_EDGE('',*,*,#5392,.T.);
#6924=ORIENTED_EDGE('',*,*,#5391,.F.);
#6925=ORIENTED_EDGE('',*,*,#5390,.T.);
#6926=ORIENTED_EDGE('',*,*,#5386,.T.);
#6927=ORIENTED_EDGE('',*,*,#5383,.T.);
#6928=ORIENTED_EDGE('',*,*,#5380,.T.);
#6929=ORIENTED_EDGE('',*,*,#5377,.T.);
#6930=ORIENTED_EDGE('',*,*,#5374,.T.);
#6931=ORIENTED_EDGE('',*,*,#5392,.F.);
#6932=ORIENTED_EDGE('',*,*,#5389,.F.);
#6933=ORIENTED_EDGE('',*,*,#5381,.T.);
#6934=ORIENTED_EDGE('',*,*,#5378,.T.);
#6935=ORIENTED_EDGE('',*,*,#5375,.T.);
#6936=ORIENTED_EDGE('',*,*,#5372,.T.);
#6937=ORIENTED_EDGE('',*,*,#5393,.F.);
#6938=ORIENTED_EDGE('',*,*,#5394,.T.);
#6939=ORIENTED_EDGE('',*,*,#5395,.F.);
#6940=ORIENTED_EDGE('',*,*,#5394,.F.);
#6941=ORIENTED_EDGE('',*,*,#5396,.F.);
#6942=ORIENTED_EDGE('',*,*,#5397,.T.);
#6943=ORIENTED_EDGE('',*,*,#5398,.F.);
#6944=ORIENTED_EDGE('',*,*,#5397,.F.);
#6945=ORIENTED_EDGE('',*,*,#5399,.F.);
#6946=ORIENTED_EDGE('',*,*,#5400,.T.);
#6947=ORIENTED_EDGE('',*,*,#5401,.F.);
#6948=ORIENTED_EDGE('',*,*,#5400,.F.);
#6949=ORIENTED_EDGE('',*,*,#5402,.F.);
#6950=ORIENTED_EDGE('',*,*,#5403,.T.);
#6951=ORIENTED_EDGE('',*,*,#5404,.F.);
#6952=ORIENTED_EDGE('',*,*,#5403,.F.);
#6953=ORIENTED_EDGE('',*,*,#5405,.F.);
#6954=ORIENTED_EDGE('',*,*,#5406,.T.);
#6955=ORIENTED_EDGE('',*,*,#5407,.T.);
#6956=ORIENTED_EDGE('',*,*,#5406,.F.);
#6957=ORIENTED_EDGE('',*,*,#5407,.F.);
#6958=ORIENTED_EDGE('',*,*,#5408,.F.);
#6959=ORIENTED_EDGE('',*,*,#5409,.F.);
#6960=ORIENTED_EDGE('',*,*,#5410,.T.);
#6961=ORIENTED_EDGE('',*,*,#5408,.T.);
#6962=ORIENTED_EDGE('',*,*,#5410,.F.);
#6963=ORIENTED_EDGE('',*,*,#5411,.F.);
#6964=ORIENTED_EDGE('',*,*,#5412,.T.);
#6965=ORIENTED_EDGE('',*,*,#5413,.T.);
#6966=ORIENTED_EDGE('',*,*,#5412,.F.);
#6967=ORIENTED_EDGE('',*,*,#5411,.T.);
#6968=ORIENTED_EDGE('',*,*,#5409,.T.);
#6969=ORIENTED_EDGE('',*,*,#5404,.T.);
#6970=ORIENTED_EDGE('',*,*,#5401,.T.);
#6971=ORIENTED_EDGE('',*,*,#5398,.T.);
#6972=ORIENTED_EDGE('',*,*,#5395,.T.);
#6973=ORIENTED_EDGE('',*,*,#5413,.F.);
#6974=ORIENTED_EDGE('',*,*,#5405,.T.);
#6975=ORIENTED_EDGE('',*,*,#5402,.T.);
#6976=ORIENTED_EDGE('',*,*,#5399,.T.);
#6977=ORIENTED_EDGE('',*,*,#5396,.T.);
#6978=ORIENTED_EDGE('',*,*,#5393,.T.);
#6979=ORIENTED_EDGE('',*,*,#5414,.T.);
#6980=ORIENTED_EDGE('',*,*,#5415,.T.);
#6981=ORIENTED_EDGE('',*,*,#5416,.T.);
#6982=ORIENTED_EDGE('',*,*,#5415,.F.);
#6983=ORIENTED_EDGE('',*,*,#5417,.F.);
#6984=ORIENTED_EDGE('',*,*,#5418,.T.);
#6985=ORIENTED_EDGE('',*,*,#5414,.F.);
#6986=ORIENTED_EDGE('',*,*,#5418,.F.);
#6987=ORIENTED_EDGE('',*,*,#5416,.F.);
#6988=ORIENTED_EDGE('',*,*,#5419,.T.);
#6989=ORIENTED_EDGE('',*,*,#5420,.T.);
#6990=ORIENTED_EDGE('',*,*,#5417,.T.);
#6991=ORIENTED_EDGE('',*,*,#5420,.F.);
#6992=ORIENTED_EDGE('',*,*,#5419,.F.);
#6993=ORIENTED_EDGE('',*,*,#5421,.F.);
#6994=ORIENTED_EDGE('',*,*,#5422,.F.);
#6995=ORIENTED_EDGE('',*,*,#5423,.T.);
#6996=ORIENTED_EDGE('',*,*,#5424,.F.);
#6997=ORIENTED_EDGE('',*,*,#5425,.F.);
#6998=ORIENTED_EDGE('',*,*,#5423,.F.);
#6999=ORIENTED_EDGE('',*,*,#5424,.T.);
#7000=ORIENTED_EDGE('',*,*,#5425,.T.);
#7001=ORIENTED_EDGE('',*,*,#5426,.T.);
#7002=ORIENTED_EDGE('',*,*,#5427,.T.);
#7003=ORIENTED_EDGE('',*,*,#5426,.F.);
#7004=ORIENTED_EDGE('',*,*,#5428,.T.);
#7005=ORIENTED_EDGE('',*,*,#5429,.T.);
#7006=ORIENTED_EDGE('',*,*,#5430,.F.);
#7007=ORIENTED_EDGE('',*,*,#5429,.F.);
#7008=ORIENTED_EDGE('',*,*,#5430,.T.);
#7009=ORIENTED_EDGE('',*,*,#5431,.T.);
#7010=ORIENTED_EDGE('',*,*,#5432,.F.);
#7011=ORIENTED_EDGE('',*,*,#5431,.F.);
#7012=ORIENTED_EDGE('',*,*,#5427,.F.);
#7013=ORIENTED_EDGE('',*,*,#5432,.T.);
#7014=ORIENTED_EDGE('',*,*,#5433,.F.);
#7015=ORIENTED_EDGE('',*,*,#5434,.T.);
#7016=ORIENTED_EDGE('',*,*,#5421,.T.);
#7017=ORIENTED_EDGE('',*,*,#5422,.T.);
#7018=ORIENTED_EDGE('',*,*,#5434,.F.);
#7019=ORIENTED_EDGE('',*,*,#5433,.T.);
#7020=ORIENTED_EDGE('',*,*,#5435,.F.);
#7021=ORIENTED_EDGE('',*,*,#5435,.T.);
#7022=ORIENTED_EDGE('',*,*,#5436,.T.);
#7023=ORIENTED_EDGE('',*,*,#5428,.F.);
#7024=ORIENTED_EDGE('',*,*,#5436,.F.);
#7025=ORIENTED_EDGE('',*,*,#5437,.F.);
#7026=ORIENTED_EDGE('',*,*,#5438,.F.);
#7027=ORIENTED_EDGE('',*,*,#5439,.T.);
#7028=ORIENTED_EDGE('',*,*,#5440,.F.);
#7029=ORIENTED_EDGE('',*,*,#5441,.F.);
#7030=ORIENTED_EDGE('',*,*,#5439,.F.);
#7031=ORIENTED_EDGE('',*,*,#5442,.T.);
#7032=ORIENTED_EDGE('',*,*,#5443,.T.);
#7033=ORIENTED_EDGE('',*,*,#5440,.T.);
#7034=ORIENTED_EDGE('',*,*,#5441,.T.);
#7035=ORIENTED_EDGE('',*,*,#5443,.F.);
#7036=ORIENTED_EDGE('',*,*,#5444,.F.);
#7037=ORIENTED_EDGE('',*,*,#5445,.T.);
#7038=ORIENTED_EDGE('',*,*,#5446,.F.);
#7039=ORIENTED_EDGE('',*,*,#5447,.T.);
#7040=ORIENTED_EDGE('',*,*,#5444,.T.);
#7041=ORIENTED_EDGE('',*,*,#5447,.F.);
#7042=ORIENTED_EDGE('',*,*,#5448,.F.);
#7043=ORIENTED_EDGE('',*,*,#5449,.T.);
#7044=ORIENTED_EDGE('',*,*,#5446,.T.);
#7045=ORIENTED_EDGE('',*,*,#5449,.F.);
#7046=ORIENTED_EDGE('',*,*,#5450,.F.);
#7047=ORIENTED_EDGE('',*,*,#5451,.T.);
#7048=ORIENTED_EDGE('',*,*,#5448,.T.);
#7049=ORIENTED_EDGE('',*,*,#5451,.F.);
#7050=ORIENTED_EDGE('',*,*,#5450,.T.);
#7051=ORIENTED_EDGE('',*,*,#5442,.F.);
#7052=ORIENTED_EDGE('',*,*,#5437,.T.);
#7053=ORIENTED_EDGE('',*,*,#5438,.T.);
#7054=ORIENTED_EDGE('',*,*,#5452,.T.);
#7055=ORIENTED_EDGE('',*,*,#5445,.F.);
#7056=ORIENTED_EDGE('',*,*,#5452,.F.);
#7057=ORIENTED_EDGE('',*,*,#5453,.T.);
#7058=ORIENTED_EDGE('',*,*,#5453,.F.);
#7059=ORIENTED_EDGE('',*,*,#5454,.T.);
#7060=ORIENTED_EDGE('',*,*,#5454,.F.);
#7061=ORIENTED_EDGE('',*,*,#5455,.T.);
#7062=ORIENTED_EDGE('',*,*,#5455,.F.);
#7063=ORIENTED_EDGE('',*,*,#5456,.T.);
#7064=ORIENTED_EDGE('',*,*,#5456,.F.);
#7065=ORIENTED_EDGE('',*,*,#5457,.T.);
#7066=ORIENTED_EDGE('',*,*,#5457,.F.);
#7067=ORIENTED_EDGE('',*,*,#5458,.T.);
#7068=ORIENTED_EDGE('',*,*,#5458,.F.);
#7069=ORIENTED_EDGE('',*,*,#5459,.T.);
#7070=ORIENTED_EDGE('',*,*,#5459,.F.);
#7071=ORIENTED_EDGE('',*,*,#5460,.F.);
#7072=ORIENTED_EDGE('',*,*,#5461,.F.);
#7073=ORIENTED_EDGE('',*,*,#5462,.F.);
#7074=ORIENTED_EDGE('',*,*,#5463,.F.);
#7075=ORIENTED_EDGE('',*,*,#5462,.T.);
#7076=ORIENTED_EDGE('',*,*,#5464,.F.);
#7077=ORIENTED_EDGE('',*,*,#5465,.T.);
#7078=ORIENTED_EDGE('',*,*,#5466,.F.);
#7079=ORIENTED_EDGE('',*,*,#5467,.T.);
#7080=ORIENTED_EDGE('',*,*,#5468,.F.);
#7081=ORIENTED_EDGE('',*,*,#5469,.T.);
#7082=ORIENTED_EDGE('',*,*,#5470,.F.);
#7083=ORIENTED_EDGE('',*,*,#5469,.F.);
#7084=ORIENTED_EDGE('',*,*,#5471,.F.);
#7085=ORIENTED_EDGE('',*,*,#5472,.T.);
#7086=ORIENTED_EDGE('',*,*,#5473,.F.);
#7087=ORIENTED_EDGE('',*,*,#5474,.T.);
#7088=ORIENTED_EDGE('',*,*,#5475,.F.);
#7089=ORIENTED_EDGE('',*,*,#5476,.T.);
#7090=ORIENTED_EDGE('',*,*,#5477,.F.);
#7091=ORIENTED_EDGE('',*,*,#5478,.T.);
#7092=ORIENTED_EDGE('',*,*,#5479,.F.);
#7093=ORIENTED_EDGE('',*,*,#5461,.T.);
#7094=ORIENTED_EDGE('',*,*,#5480,.T.);
#7095=ORIENTED_EDGE('',*,*,#5481,.T.);
#7096=ORIENTED_EDGE('',*,*,#5464,.T.);
#7097=ORIENTED_EDGE('',*,*,#5482,.F.);
#7098=ORIENTED_EDGE('',*,*,#5483,.F.);
#7099=ORIENTED_EDGE('',*,*,#5465,.F.);
#7100=ORIENTED_EDGE('',*,*,#5481,.F.);
#7101=ORIENTED_EDGE('',*,*,#5483,.T.);
#7102=ORIENTED_EDGE('',*,*,#5484,.T.);
#7103=ORIENTED_EDGE('',*,*,#5485,.T.);
#7104=ORIENTED_EDGE('',*,*,#5466,.T.);
#7105=ORIENTED_EDGE('',*,*,#5486,.F.);
#7106=ORIENTED_EDGE('',*,*,#5487,.F.);
#7107=ORIENTED_EDGE('',*,*,#5467,.F.);
#7108=ORIENTED_EDGE('',*,*,#5485,.F.);
#7109=ORIENTED_EDGE('',*,*,#5487,.T.);
#7110=ORIENTED_EDGE('',*,*,#5488,.T.);
#7111=ORIENTED_EDGE('',*,*,#5489,.T.);
#7112=ORIENTED_EDGE('',*,*,#5490,.T.);
#7113=ORIENTED_EDGE('',*,*,#5471,.T.);
#7114=ORIENTED_EDGE('',*,*,#5468,.T.);
#7115=ORIENTED_EDGE('',*,*,#5491,.F.);
#7116=ORIENTED_EDGE('',*,*,#5492,.F.);
#7117=ORIENTED_EDGE('',*,*,#5472,.F.);
#7118=ORIENTED_EDGE('',*,*,#5490,.F.);
#7119=ORIENTED_EDGE('',*,*,#5492,.T.);
#7120=ORIENTED_EDGE('',*,*,#5493,.T.);
#7121=ORIENTED_EDGE('',*,*,#5494,.T.);
#7122=ORIENTED_EDGE('',*,*,#5473,.T.);
#7123=ORIENTED_EDGE('',*,*,#5495,.F.);
#7124=ORIENTED_EDGE('',*,*,#5496,.F.);
#7125=ORIENTED_EDGE('',*,*,#5474,.F.);
#7126=ORIENTED_EDGE('',*,*,#5494,.F.);
#7127=ORIENTED_EDGE('',*,*,#5496,.T.);
#7128=ORIENTED_EDGE('',*,*,#5497,.T.);
#7129=ORIENTED_EDGE('',*,*,#5498,.T.);
#7130=ORIENTED_EDGE('',*,*,#5475,.T.);
#7131=ORIENTED_EDGE('',*,*,#5476,.F.);
#7132=ORIENTED_EDGE('',*,*,#5498,.F.);
#7133=ORIENTED_EDGE('',*,*,#5499,.F.);
#7134=ORIENTED_EDGE('',*,*,#5500,.F.);
#7135=ORIENTED_EDGE('',*,*,#5501,.F.);
#7136=ORIENTED_EDGE('',*,*,#5502,.T.);
#7137=ORIENTED_EDGE('',*,*,#5488,.F.);
#7138=ORIENTED_EDGE('',*,*,#5486,.T.);
#7139=ORIENTED_EDGE('',*,*,#5484,.F.);
#7140=ORIENTED_EDGE('',*,*,#5482,.T.);
#7141=ORIENTED_EDGE('',*,*,#5480,.F.);
#7142=ORIENTED_EDGE('',*,*,#5460,.T.);
#7143=ORIENTED_EDGE('',*,*,#5503,.F.);
#7144=ORIENTED_EDGE('',*,*,#5504,.T.);
#7145=ORIENTED_EDGE('',*,*,#5505,.F.);
#7146=ORIENTED_EDGE('',*,*,#5499,.T.);
#7147=ORIENTED_EDGE('',*,*,#5497,.F.);
#7148=ORIENTED_EDGE('',*,*,#5495,.T.);
#7149=ORIENTED_EDGE('',*,*,#5493,.F.);
#7150=ORIENTED_EDGE('',*,*,#5491,.T.);
#7151=ORIENTED_EDGE('',*,*,#5489,.F.);
#7152=ORIENTED_EDGE('',*,*,#5502,.F.);
#7153=ORIENTED_EDGE('',*,*,#5463,.T.);
#7154=ORIENTED_EDGE('',*,*,#5479,.T.);
#7155=ORIENTED_EDGE('',*,*,#5506,.T.);
#7156=ORIENTED_EDGE('',*,*,#5503,.T.);
#7157=ORIENTED_EDGE('',*,*,#5478,.F.);
#7158=ORIENTED_EDGE('',*,*,#5507,.F.);
#7159=ORIENTED_EDGE('',*,*,#5504,.F.);
#7160=ORIENTED_EDGE('',*,*,#5506,.F.);
#7161=ORIENTED_EDGE('',*,*,#5470,.T.);
#7162=ORIENTED_EDGE('',*,*,#5501,.T.);
#7163=ORIENTED_EDGE('',*,*,#5500,.T.);
#7164=ORIENTED_EDGE('',*,*,#5505,.T.);
#7165=ORIENTED_EDGE('',*,*,#5507,.T.);
#7166=ORIENTED_EDGE('',*,*,#5477,.T.);
#7167=ORIENTED_EDGE('',*,*,#5508,.F.);
#7168=ORIENTED_EDGE('',*,*,#5509,.T.);
#7169=ORIENTED_EDGE('',*,*,#5510,.F.);
#7170=ORIENTED_EDGE('',*,*,#5511,.T.);
#7171=ORIENTED_EDGE('',*,*,#5508,.T.);
#7172=ORIENTED_EDGE('',*,*,#5511,.F.);
#7173=ORIENTED_EDGE('',*,*,#5510,.T.);
#7174=ORIENTED_EDGE('',*,*,#5512,.F.);
#7175=ORIENTED_EDGE('',*,*,#5512,.T.);
#7176=ORIENTED_EDGE('',*,*,#5513,.T.);
#7177=ORIENTED_EDGE('',*,*,#5509,.F.);
#7178=ORIENTED_EDGE('',*,*,#5513,.F.);
#7179=ORIENTED_EDGE('',*,*,#5514,.F.);
#7180=ORIENTED_EDGE('',*,*,#5515,.T.);
#7181=ORIENTED_EDGE('',*,*,#5516,.F.);
#7182=ORIENTED_EDGE('',*,*,#5517,.T.);
#7183=ORIENTED_EDGE('',*,*,#5514,.T.);
#7184=ORIENTED_EDGE('',*,*,#5517,.F.);
#7185=ORIENTED_EDGE('',*,*,#5516,.T.);
#7186=ORIENTED_EDGE('',*,*,#5518,.F.);
#7187=ORIENTED_EDGE('',*,*,#5518,.T.);
#7188=ORIENTED_EDGE('',*,*,#5519,.T.);
#7189=ORIENTED_EDGE('',*,*,#5515,.F.);
#7190=ORIENTED_EDGE('',*,*,#5519,.F.);
#7191=ORIENTED_EDGE('',*,*,#5520,.F.);
#7192=ORIENTED_EDGE('',*,*,#5521,.T.);
#7193=ORIENTED_EDGE('',*,*,#5522,.F.);
#7194=ORIENTED_EDGE('',*,*,#5521,.F.);
#7195=ORIENTED_EDGE('',*,*,#5520,.T.);
#7196=ORIENTED_EDGE('',*,*,#5523,.F.);
#7197=ORIENTED_EDGE('',*,*,#5524,.T.);
#7198=ORIENTED_EDGE('',*,*,#5525,.F.);
#7199=ORIENTED_EDGE('',*,*,#5524,.F.);
#7200=ORIENTED_EDGE('',*,*,#5523,.T.);
#7201=ORIENTED_EDGE('',*,*,#5526,.F.);
#7202=ORIENTED_EDGE('',*,*,#5527,.T.);
#7203=ORIENTED_EDGE('',*,*,#5528,.F.);
#7204=ORIENTED_EDGE('',*,*,#5527,.F.);
#7205=ORIENTED_EDGE('',*,*,#5526,.T.);
#7206=ORIENTED_EDGE('',*,*,#5529,.F.);
#7207=ORIENTED_EDGE('',*,*,#5530,.T.);
#7208=ORIENTED_EDGE('',*,*,#5531,.F.);
#7209=ORIENTED_EDGE('',*,*,#5530,.F.);
#7210=ORIENTED_EDGE('',*,*,#5529,.T.);
#7211=ORIENTED_EDGE('',*,*,#5532,.F.);
#7212=ORIENTED_EDGE('',*,*,#5533,.T.);
#7213=ORIENTED_EDGE('',*,*,#5534,.F.);
#7214=ORIENTED_EDGE('',*,*,#5533,.F.);
#7215=ORIENTED_EDGE('',*,*,#5532,.T.);
#7216=ORIENTED_EDGE('',*,*,#5535,.F.);
#7217=ORIENTED_EDGE('',*,*,#5536,.T.);
#7218=ORIENTED_EDGE('',*,*,#5537,.F.);
#7219=ORIENTED_EDGE('',*,*,#5536,.F.);
#7220=ORIENTED_EDGE('',*,*,#5535,.T.);
#7221=ORIENTED_EDGE('',*,*,#5538,.F.);
#7222=ORIENTED_EDGE('',*,*,#5539,.T.);
#7223=ORIENTED_EDGE('',*,*,#5540,.F.);
#7224=ORIENTED_EDGE('',*,*,#5539,.F.);
#7225=ORIENTED_EDGE('',*,*,#5541,.F.);
#7226=ORIENTED_EDGE('',*,*,#5542,.T.);
#7227=ORIENTED_EDGE('',*,*,#5543,.F.);
#7228=ORIENTED_EDGE('',*,*,#5542,.F.);
#7229=ORIENTED_EDGE('',*,*,#5544,.F.);
#7230=ORIENTED_EDGE('',*,*,#5545,.T.);
#7231=ORIENTED_EDGE('',*,*,#5546,.F.);
#7232=ORIENTED_EDGE('',*,*,#5545,.F.);
#7233=ORIENTED_EDGE('',*,*,#5547,.F.);
#7234=ORIENTED_EDGE('',*,*,#5548,.T.);
#7235=ORIENTED_EDGE('',*,*,#5549,.F.);
#7236=ORIENTED_EDGE('',*,*,#5548,.F.);
#7237=ORIENTED_EDGE('',*,*,#5550,.F.);
#7238=ORIENTED_EDGE('',*,*,#5551,.T.);
#7239=ORIENTED_EDGE('',*,*,#5552,.F.);
#7240=ORIENTED_EDGE('',*,*,#5551,.F.);
#7241=ORIENTED_EDGE('',*,*,#5553,.F.);
#7242=ORIENTED_EDGE('',*,*,#5554,.T.);
#7243=ORIENTED_EDGE('',*,*,#5555,.F.);
#7244=ORIENTED_EDGE('',*,*,#5554,.F.);
#7245=ORIENTED_EDGE('',*,*,#5556,.F.);
#7246=ORIENTED_EDGE('',*,*,#5557,.T.);
#7247=ORIENTED_EDGE('',*,*,#5558,.F.);
#7248=ORIENTED_EDGE('',*,*,#5557,.F.);
#7249=ORIENTED_EDGE('',*,*,#5559,.T.);
#7250=ORIENTED_EDGE('',*,*,#5560,.T.);
#7251=ORIENTED_EDGE('',*,*,#5561,.F.);
#7252=ORIENTED_EDGE('',*,*,#5562,.F.);
#7253=ORIENTED_EDGE('',*,*,#5563,.T.);
#7254=ORIENTED_EDGE('',*,*,#5562,.T.);
#7255=ORIENTED_EDGE('',*,*,#5564,.F.);
#7256=ORIENTED_EDGE('',*,*,#5565,.F.);
#7257=ORIENTED_EDGE('',*,*,#5534,.T.);
#7258=ORIENTED_EDGE('',*,*,#5537,.T.);
#7259=ORIENTED_EDGE('',*,*,#5558,.T.);
#7260=ORIENTED_EDGE('',*,*,#5555,.T.);
#7261=ORIENTED_EDGE('',*,*,#5552,.T.);
#7262=ORIENTED_EDGE('',*,*,#5549,.T.);
#7263=ORIENTED_EDGE('',*,*,#5546,.T.);
#7264=ORIENTED_EDGE('',*,*,#5543,.T.);
#7265=ORIENTED_EDGE('',*,*,#5540,.T.);
#7266=ORIENTED_EDGE('',*,*,#5531,.T.);
#7267=ORIENTED_EDGE('',*,*,#5528,.T.);
#7268=ORIENTED_EDGE('',*,*,#5525,.T.);
#7269=ORIENTED_EDGE('',*,*,#5522,.T.);
#7270=ORIENTED_EDGE('',*,*,#5566,.T.);
#7271=ORIENTED_EDGE('',*,*,#5565,.T.);
#7272=ORIENTED_EDGE('',*,*,#5567,.F.);
#7273=ORIENTED_EDGE('',*,*,#5568,.F.);
#7274=ORIENTED_EDGE('',*,*,#5569,.T.);
#7275=ORIENTED_EDGE('',*,*,#5568,.T.);
#7276=ORIENTED_EDGE('',*,*,#5570,.F.);
#7277=ORIENTED_EDGE('',*,*,#5560,.F.);
#7278=ORIENTED_EDGE('',*,*,#5556,.T.);
#7279=ORIENTED_EDGE('',*,*,#5553,.T.);
#7280=ORIENTED_EDGE('',*,*,#5550,.T.);
#7281=ORIENTED_EDGE('',*,*,#5547,.T.);
#7282=ORIENTED_EDGE('',*,*,#5544,.T.);
#7283=ORIENTED_EDGE('',*,*,#5541,.T.);
#7284=ORIENTED_EDGE('',*,*,#5538,.T.);
#7285=ORIENTED_EDGE('',*,*,#5570,.T.);
#7286=ORIENTED_EDGE('',*,*,#5567,.T.);
#7287=ORIENTED_EDGE('',*,*,#5564,.T.);
#7288=ORIENTED_EDGE('',*,*,#5561,.T.);
#7289=ORIENTED_EDGE('',*,*,#5569,.F.);
#7290=ORIENTED_EDGE('',*,*,#5559,.F.);
#7291=ORIENTED_EDGE('',*,*,#5563,.F.);
#7292=ORIENTED_EDGE('',*,*,#5566,.F.);
#7293=ORIENTED_EDGE('',*,*,#5571,.F.);
#7294=ORIENTED_EDGE('',*,*,#5572,.T.);
#7295=ORIENTED_EDGE('',*,*,#5573,.F.);
#7296=ORIENTED_EDGE('',*,*,#5572,.F.);
#7297=ORIENTED_EDGE('',*,*,#5574,.F.);
#7298=ORIENTED_EDGE('',*,*,#5575,.T.);
#7299=ORIENTED_EDGE('',*,*,#5576,.F.);
#7300=ORIENTED_EDGE('',*,*,#5575,.F.);
#7301=ORIENTED_EDGE('',*,*,#5577,.F.);
#7302=ORIENTED_EDGE('',*,*,#5578,.T.);
#7303=ORIENTED_EDGE('',*,*,#5579,.F.);
#7304=ORIENTED_EDGE('',*,*,#5578,.F.);
#7305=ORIENTED_EDGE('',*,*,#5580,.F.);
#7306=ORIENTED_EDGE('',*,*,#5581,.T.);
#7307=ORIENTED_EDGE('',*,*,#5582,.F.);
#7308=ORIENTED_EDGE('',*,*,#5581,.F.);
#7309=ORIENTED_EDGE('',*,*,#5583,.F.);
#7310=ORIENTED_EDGE('',*,*,#5584,.T.);
#7311=ORIENTED_EDGE('',*,*,#5585,.F.);
#7312=ORIENTED_EDGE('',*,*,#5584,.F.);
#7313=ORIENTED_EDGE('',*,*,#5586,.F.);
#7314=ORIENTED_EDGE('',*,*,#5587,.T.);
#7315=ORIENTED_EDGE('',*,*,#5588,.F.);
#7316=ORIENTED_EDGE('',*,*,#5587,.F.);
#7317=ORIENTED_EDGE('',*,*,#5589,.F.);
#7318=ORIENTED_EDGE('',*,*,#5590,.T.);
#7319=ORIENTED_EDGE('',*,*,#5591,.F.);
#7320=ORIENTED_EDGE('',*,*,#5590,.F.);
#7321=ORIENTED_EDGE('',*,*,#5592,.T.);
#7322=ORIENTED_EDGE('',*,*,#5593,.T.);
#7323=ORIENTED_EDGE('',*,*,#5594,.F.);
#7324=ORIENTED_EDGE('',*,*,#5595,.F.);
#7325=ORIENTED_EDGE('',*,*,#5596,.T.);
#7326=ORIENTED_EDGE('',*,*,#5595,.T.);
#7327=ORIENTED_EDGE('',*,*,#5597,.F.);
#7328=ORIENTED_EDGE('',*,*,#5598,.F.);
#7329=ORIENTED_EDGE('',*,*,#5591,.T.);
#7330=ORIENTED_EDGE('',*,*,#5588,.T.);
#7331=ORIENTED_EDGE('',*,*,#5585,.T.);
#7332=ORIENTED_EDGE('',*,*,#5582,.T.);
#7333=ORIENTED_EDGE('',*,*,#5579,.T.);
#7334=ORIENTED_EDGE('',*,*,#5576,.T.);
#7335=ORIENTED_EDGE('',*,*,#5573,.T.);
#7336=ORIENTED_EDGE('',*,*,#5599,.T.);
#7337=ORIENTED_EDGE('',*,*,#5598,.T.);
#7338=ORIENTED_EDGE('',*,*,#5600,.F.);
#7339=ORIENTED_EDGE('',*,*,#5601,.F.);
#7340=ORIENTED_EDGE('',*,*,#5602,.T.);
#7341=ORIENTED_EDGE('',*,*,#5601,.T.);
#7342=ORIENTED_EDGE('',*,*,#5603,.F.);
#7343=ORIENTED_EDGE('',*,*,#5593,.F.);
#7344=ORIENTED_EDGE('',*,*,#5589,.T.);
#7345=ORIENTED_EDGE('',*,*,#5586,.T.);
#7346=ORIENTED_EDGE('',*,*,#5583,.T.);
#7347=ORIENTED_EDGE('',*,*,#5580,.T.);
#7348=ORIENTED_EDGE('',*,*,#5577,.T.);
#7349=ORIENTED_EDGE('',*,*,#5574,.T.);
#7350=ORIENTED_EDGE('',*,*,#5571,.T.);
#7351=ORIENTED_EDGE('',*,*,#5603,.T.);
#7352=ORIENTED_EDGE('',*,*,#5600,.T.);
#7353=ORIENTED_EDGE('',*,*,#5597,.T.);
#7354=ORIENTED_EDGE('',*,*,#5594,.T.);
#7355=ORIENTED_EDGE('',*,*,#5602,.F.);
#7356=ORIENTED_EDGE('',*,*,#5592,.F.);
#7357=ORIENTED_EDGE('',*,*,#5596,.F.);
#7358=ORIENTED_EDGE('',*,*,#5599,.F.);
#7359=ORIENTED_EDGE('',*,*,#5604,.F.);
#7360=ORIENTED_EDGE('',*,*,#5605,.T.);
#7361=ORIENTED_EDGE('',*,*,#5606,.F.);
#7362=ORIENTED_EDGE('',*,*,#5605,.F.);
#7363=ORIENTED_EDGE('',*,*,#5607,.F.);
#7364=ORIENTED_EDGE('',*,*,#5608,.T.);
#7365=ORIENTED_EDGE('',*,*,#5609,.F.);
#7366=ORIENTED_EDGE('',*,*,#5608,.F.);
#7367=ORIENTED_EDGE('',*,*,#5610,.F.);
#7368=ORIENTED_EDGE('',*,*,#5611,.T.);
#7369=ORIENTED_EDGE('',*,*,#5612,.F.);
#7370=ORIENTED_EDGE('',*,*,#5611,.F.);
#7371=ORIENTED_EDGE('',*,*,#5613,.F.);
#7372=ORIENTED_EDGE('',*,*,#5614,.T.);
#7373=ORIENTED_EDGE('',*,*,#5615,.F.);
#7374=ORIENTED_EDGE('',*,*,#5614,.F.);
#7375=ORIENTED_EDGE('',*,*,#5616,.F.);
#7376=ORIENTED_EDGE('',*,*,#5617,.T.);
#7377=ORIENTED_EDGE('',*,*,#5618,.F.);
#7378=ORIENTED_EDGE('',*,*,#5617,.F.);
#7379=ORIENTED_EDGE('',*,*,#5619,.F.);
#7380=ORIENTED_EDGE('',*,*,#5620,.T.);
#7381=ORIENTED_EDGE('',*,*,#5621,.F.);
#7382=ORIENTED_EDGE('',*,*,#5620,.F.);
#7383=ORIENTED_EDGE('',*,*,#5622,.F.);
#7384=ORIENTED_EDGE('',*,*,#5623,.T.);
#7385=ORIENTED_EDGE('',*,*,#5624,.F.);
#7386=ORIENTED_EDGE('',*,*,#5623,.F.);
#7387=ORIENTED_EDGE('',*,*,#5625,.T.);
#7388=ORIENTED_EDGE('',*,*,#5626,.T.);
#7389=ORIENTED_EDGE('',*,*,#5627,.F.);
#7390=ORIENTED_EDGE('',*,*,#5628,.F.);
#7391=ORIENTED_EDGE('',*,*,#5629,.T.);
#7392=ORIENTED_EDGE('',*,*,#5628,.T.);
#7393=ORIENTED_EDGE('',*,*,#5630,.F.);
#7394=ORIENTED_EDGE('',*,*,#5631,.F.);
#7395=ORIENTED_EDGE('',*,*,#5624,.T.);
#7396=ORIENTED_EDGE('',*,*,#5621,.T.);
#7397=ORIENTED_EDGE('',*,*,#5618,.T.);
#7398=ORIENTED_EDGE('',*,*,#5615,.T.);
#7399=ORIENTED_EDGE('',*,*,#5612,.T.);
#7400=ORIENTED_EDGE('',*,*,#5609,.T.);
#7401=ORIENTED_EDGE('',*,*,#5606,.T.);
#7402=ORIENTED_EDGE('',*,*,#5632,.T.);
#7403=ORIENTED_EDGE('',*,*,#5631,.T.);
#7404=ORIENTED_EDGE('',*,*,#5633,.F.);
#7405=ORIENTED_EDGE('',*,*,#5634,.F.);
#7406=ORIENTED_EDGE('',*,*,#5635,.T.);
#7407=ORIENTED_EDGE('',*,*,#5634,.T.);
#7408=ORIENTED_EDGE('',*,*,#5636,.F.);
#7409=ORIENTED_EDGE('',*,*,#5626,.F.);
#7410=ORIENTED_EDGE('',*,*,#5622,.T.);
#7411=ORIENTED_EDGE('',*,*,#5619,.T.);
#7412=ORIENTED_EDGE('',*,*,#5616,.T.);
#7413=ORIENTED_EDGE('',*,*,#5613,.T.);
#7414=ORIENTED_EDGE('',*,*,#5610,.T.);
#7415=ORIENTED_EDGE('',*,*,#5607,.T.);
#7416=ORIENTED_EDGE('',*,*,#5604,.T.);
#7417=ORIENTED_EDGE('',*,*,#5636,.T.);
#7418=ORIENTED_EDGE('',*,*,#5633,.T.);
#7419=ORIENTED_EDGE('',*,*,#5630,.T.);
#7420=ORIENTED_EDGE('',*,*,#5627,.T.);
#7421=ORIENTED_EDGE('',*,*,#5635,.F.);
#7422=ORIENTED_EDGE('',*,*,#5625,.F.);
#7423=ORIENTED_EDGE('',*,*,#5629,.F.);
#7424=ORIENTED_EDGE('',*,*,#5632,.F.);
#7425=ORIENTED_EDGE('',*,*,#5637,.F.);
#7426=ORIENTED_EDGE('',*,*,#5638,.T.);
#7427=ORIENTED_EDGE('',*,*,#5639,.T.);
#7428=ORIENTED_EDGE('',*,*,#5640,.F.);
#7429=ORIENTED_EDGE('',*,*,#5641,.F.);
#7430=ORIENTED_EDGE('',*,*,#5642,.F.);
#7431=ORIENTED_EDGE('',*,*,#5639,.F.);
#7432=ORIENTED_EDGE('',*,*,#5643,.T.);
#7433=ORIENTED_EDGE('',*,*,#5644,.F.);
#7434=ORIENTED_EDGE('',*,*,#5643,.F.);
#7435=ORIENTED_EDGE('',*,*,#5638,.F.);
#7436=ORIENTED_EDGE('',*,*,#5645,.F.);
#7437=ORIENTED_EDGE('',*,*,#5646,.T.);
#7438=ORIENTED_EDGE('',*,*,#5647,.F.);
#7439=ORIENTED_EDGE('',*,*,#5648,.F.);
#7440=ORIENTED_EDGE('',*,*,#5649,.F.);
#7441=ORIENTED_EDGE('',*,*,#5650,.T.);
#7442=ORIENTED_EDGE('',*,*,#5651,.F.);
#7443=ORIENTED_EDGE('',*,*,#5650,.F.);
#7444=ORIENTED_EDGE('',*,*,#5652,.F.);
#7445=ORIENTED_EDGE('',*,*,#5653,.F.);
#7446=ORIENTED_EDGE('',*,*,#5646,.F.);
#7447=ORIENTED_EDGE('',*,*,#5640,.T.);
#7448=ORIENTED_EDGE('',*,*,#5637,.T.);
#7449=ORIENTED_EDGE('',*,*,#5642,.T.);
#7450=ORIENTED_EDGE('',*,*,#5654,.F.);
#7451=ORIENTED_EDGE('',*,*,#5648,.T.);
#7452=ORIENTED_EDGE('',*,*,#5645,.T.);
#7453=ORIENTED_EDGE('',*,*,#5655,.T.);
#7454=ORIENTED_EDGE('',*,*,#5656,.T.);
#7455=ORIENTED_EDGE('',*,*,#5655,.F.);
#7456=ORIENTED_EDGE('',*,*,#5647,.T.);
#7457=ORIENTED_EDGE('',*,*,#5653,.T.);
#7458=ORIENTED_EDGE('',*,*,#5657,.F.);
#7459=ORIENTED_EDGE('',*,*,#5658,.F.);
#7460=ORIENTED_EDGE('',*,*,#5641,.T.);
#7461=ORIENTED_EDGE('',*,*,#5657,.T.);
#7462=ORIENTED_EDGE('',*,*,#5652,.T.);
#7463=ORIENTED_EDGE('',*,*,#5649,.T.);
#7464=ORIENTED_EDGE('',*,*,#5654,.T.);
#7465=ORIENTED_EDGE('',*,*,#5659,.F.);
#7466=ORIENTED_EDGE('',*,*,#5660,.T.);
#7467=ORIENTED_EDGE('',*,*,#5658,.T.);
#7468=ORIENTED_EDGE('',*,*,#5660,.F.);
#7469=ORIENTED_EDGE('',*,*,#5659,.T.);
#7470=ORIENTED_EDGE('',*,*,#5644,.T.);
#7471=ORIENTED_EDGE('',*,*,#5651,.T.);
#7472=ORIENTED_EDGE('',*,*,#5661,.T.);
#7473=ORIENTED_EDGE('',*,*,#5661,.F.);
#7474=ORIENTED_EDGE('',*,*,#5662,.T.);
#7475=ORIENTED_EDGE('',*,*,#5663,.T.);
#7476=ORIENTED_EDGE('',*,*,#5662,.F.);
#7477=ORIENTED_EDGE('',*,*,#5656,.F.);
#7478=ORIENTED_EDGE('',*,*,#5663,.F.);
#7479=ORIENTED_EDGE('',*,*,#5664,.F.);
#7480=ORIENTED_EDGE('',*,*,#5665,.T.);
#7481=ORIENTED_EDGE('',*,*,#5666,.F.);
#7482=ORIENTED_EDGE('',*,*,#5665,.F.);
#7483=ORIENTED_EDGE('',*,*,#5664,.T.);
#7484=ORIENTED_EDGE('',*,*,#5667,.F.);
#7485=ORIENTED_EDGE('',*,*,#5668,.F.);
#7486=ORIENTED_EDGE('',*,*,#5669,.T.);
#7487=ORIENTED_EDGE('',*,*,#5670,.F.);
#7488=ORIENTED_EDGE('',*,*,#5669,.F.);
#7489=ORIENTED_EDGE('',*,*,#5668,.T.);
#7490=ORIENTED_EDGE('',*,*,#5671,.F.);
#7491=ORIENTED_EDGE('',*,*,#5672,.F.);
#7492=ORIENTED_EDGE('',*,*,#5673,.T.);
#7493=ORIENTED_EDGE('',*,*,#5674,.F.);
#7494=ORIENTED_EDGE('',*,*,#5673,.F.);
#7495=ORIENTED_EDGE('',*,*,#5672,.T.);
#7496=ORIENTED_EDGE('',*,*,#5675,.F.);
#7497=ORIENTED_EDGE('',*,*,#5676,.F.);
#7498=ORIENTED_EDGE('',*,*,#5677,.T.);
#7499=ORIENTED_EDGE('',*,*,#5678,.F.);
#7500=ORIENTED_EDGE('',*,*,#5677,.F.);
#7501=ORIENTED_EDGE('',*,*,#5676,.T.);
#7502=ORIENTED_EDGE('',*,*,#5679,.F.);
#7503=ORIENTED_EDGE('',*,*,#5680,.F.);
#7504=ORIENTED_EDGE('',*,*,#5681,.T.);
#7505=ORIENTED_EDGE('',*,*,#5667,.T.);
#7506=ORIENTED_EDGE('',*,*,#5681,.F.);
#7507=ORIENTED_EDGE('',*,*,#5682,.F.);
#7508=ORIENTED_EDGE('',*,*,#5683,.T.);
#7509=ORIENTED_EDGE('',*,*,#5671,.T.);
#7510=ORIENTED_EDGE('',*,*,#5683,.F.);
#7511=ORIENTED_EDGE('',*,*,#5684,.F.);
#7512=ORIENTED_EDGE('',*,*,#5685,.T.);
#7513=ORIENTED_EDGE('',*,*,#5675,.T.);
#7514=ORIENTED_EDGE('',*,*,#5685,.F.);
#7515=ORIENTED_EDGE('',*,*,#5686,.F.);
#7516=ORIENTED_EDGE('',*,*,#5687,.T.);
#7517=ORIENTED_EDGE('',*,*,#5679,.T.);
#7518=ORIENTED_EDGE('',*,*,#5687,.F.);
#7519=ORIENTED_EDGE('',*,*,#5688,.T.);
#7520=ORIENTED_EDGE('',*,*,#5689,.T.);
#7521=ORIENTED_EDGE('',*,*,#5690,.F.);
#7522=ORIENTED_EDGE('',*,*,#5691,.F.);
#7523=ORIENTED_EDGE('',*,*,#5692,.T.);
#7524=ORIENTED_EDGE('',*,*,#5691,.T.);
#7525=ORIENTED_EDGE('',*,*,#5693,.F.);
#7526=ORIENTED_EDGE('',*,*,#5694,.F.);
#7527=ORIENTED_EDGE('',*,*,#5678,.T.);
#7528=ORIENTED_EDGE('',*,*,#5674,.T.);
#7529=ORIENTED_EDGE('',*,*,#5670,.T.);
#7530=ORIENTED_EDGE('',*,*,#5666,.T.);
#7531=ORIENTED_EDGE('',*,*,#5695,.T.);
#7532=ORIENTED_EDGE('',*,*,#5694,.T.);
#7533=ORIENTED_EDGE('',*,*,#5696,.F.);
#7534=ORIENTED_EDGE('',*,*,#5697,.F.);
#7535=ORIENTED_EDGE('',*,*,#5698,.T.);
#7536=ORIENTED_EDGE('',*,*,#5697,.T.);
#7537=ORIENTED_EDGE('',*,*,#5699,.F.);
#7538=ORIENTED_EDGE('',*,*,#5689,.F.);
#7539=ORIENTED_EDGE('',*,*,#5680,.T.);
#7540=ORIENTED_EDGE('',*,*,#5682,.T.);
#7541=ORIENTED_EDGE('',*,*,#5684,.T.);
#7542=ORIENTED_EDGE('',*,*,#5686,.T.);
#7543=ORIENTED_EDGE('',*,*,#5699,.T.);
#7544=ORIENTED_EDGE('',*,*,#5696,.T.);
#7545=ORIENTED_EDGE('',*,*,#5693,.T.);
#7546=ORIENTED_EDGE('',*,*,#5690,.T.);
#7547=ORIENTED_EDGE('',*,*,#5698,.F.);
#7548=ORIENTED_EDGE('',*,*,#5688,.F.);
#7549=ORIENTED_EDGE('',*,*,#5692,.F.);
#7550=ORIENTED_EDGE('',*,*,#5695,.F.);
#7551=ORIENTED_EDGE('',*,*,#5700,.F.);
#7552=ORIENTED_EDGE('',*,*,#5701,.T.);
#7553=ORIENTED_EDGE('',*,*,#5702,.T.);
#7554=ORIENTED_EDGE('',*,*,#5701,.F.);
#7555=ORIENTED_EDGE('',*,*,#5702,.F.);
#7556=ORIENTED_EDGE('',*,*,#5703,.F.);
#7557=ORIENTED_EDGE('',*,*,#5704,.T.);
#7558=ORIENTED_EDGE('',*,*,#5705,.T.);
#7559=ORIENTED_EDGE('',*,*,#5704,.F.);
#7560=ORIENTED_EDGE('',*,*,#5705,.F.);
#7561=ORIENTED_EDGE('',*,*,#5706,.F.);
#7562=ORIENTED_EDGE('',*,*,#5707,.T.);
#7563=ORIENTED_EDGE('',*,*,#5708,.T.);
#7564=ORIENTED_EDGE('',*,*,#5707,.F.);
#7565=ORIENTED_EDGE('',*,*,#5708,.F.);
#7566=ORIENTED_EDGE('',*,*,#5709,.F.);
#7567=ORIENTED_EDGE('',*,*,#5710,.T.);
#7568=ORIENTED_EDGE('',*,*,#5711,.T.);
#7569=ORIENTED_EDGE('',*,*,#5710,.F.);
#7570=ORIENTED_EDGE('',*,*,#5711,.F.);
#7571=ORIENTED_EDGE('',*,*,#5712,.F.);
#7572=ORIENTED_EDGE('',*,*,#5713,.T.);
#7573=ORIENTED_EDGE('',*,*,#5714,.T.);
#7574=ORIENTED_EDGE('',*,*,#5713,.F.);
#7575=ORIENTED_EDGE('',*,*,#5714,.F.);
#7576=ORIENTED_EDGE('',*,*,#5715,.F.);
#7577=ORIENTED_EDGE('',*,*,#5716,.T.);
#7578=ORIENTED_EDGE('',*,*,#5717,.T.);
#7579=ORIENTED_EDGE('',*,*,#5716,.F.);
#7580=ORIENTED_EDGE('',*,*,#5717,.F.);
#7581=ORIENTED_EDGE('',*,*,#5718,.F.);
#7582=ORIENTED_EDGE('',*,*,#5719,.T.);
#7583=ORIENTED_EDGE('',*,*,#5720,.F.);
#7584=ORIENTED_EDGE('',*,*,#5719,.F.);
#7585=ORIENTED_EDGE('',*,*,#5721,.F.);
#7586=ORIENTED_EDGE('',*,*,#5722,.T.);
#7587=ORIENTED_EDGE('',*,*,#5723,.F.);
#7588=ORIENTED_EDGE('',*,*,#5722,.F.);
#7589=ORIENTED_EDGE('',*,*,#5724,.F.);
#7590=ORIENTED_EDGE('',*,*,#5725,.T.);
#7591=ORIENTED_EDGE('',*,*,#5726,.F.);
#7592=ORIENTED_EDGE('',*,*,#5725,.F.);
#7593=ORIENTED_EDGE('',*,*,#5727,.F.);
#7594=ORIENTED_EDGE('',*,*,#5728,.T.);
#7595=ORIENTED_EDGE('',*,*,#5729,.F.);
#7596=ORIENTED_EDGE('',*,*,#5728,.F.);
#7597=ORIENTED_EDGE('',*,*,#5730,.F.);
#7598=ORIENTED_EDGE('',*,*,#5731,.T.);
#7599=ORIENTED_EDGE('',*,*,#5732,.F.);
#7600=ORIENTED_EDGE('',*,*,#5731,.F.);
#7601=ORIENTED_EDGE('',*,*,#5733,.F.);
#7602=ORIENTED_EDGE('',*,*,#5734,.T.);
#7603=ORIENTED_EDGE('',*,*,#5735,.F.);
#7604=ORIENTED_EDGE('',*,*,#5734,.F.);
#7605=ORIENTED_EDGE('',*,*,#5736,.F.);
#7606=ORIENTED_EDGE('',*,*,#5737,.T.);
#7607=ORIENTED_EDGE('',*,*,#5738,.F.);
#7608=ORIENTED_EDGE('',*,*,#5737,.F.);
#7609=ORIENTED_EDGE('',*,*,#5739,.T.);
#7610=ORIENTED_EDGE('',*,*,#5740,.T.);
#7611=ORIENTED_EDGE('',*,*,#5741,.F.);
#7612=ORIENTED_EDGE('',*,*,#5742,.F.);
#7613=ORIENTED_EDGE('',*,*,#5743,.T.);
#7614=ORIENTED_EDGE('',*,*,#5742,.T.);
#7615=ORIENTED_EDGE('',*,*,#5744,.F.);
#7616=ORIENTED_EDGE('',*,*,#5745,.F.);
#7617=ORIENTED_EDGE('',*,*,#5738,.T.);
#7618=ORIENTED_EDGE('',*,*,#5735,.T.);
#7619=ORIENTED_EDGE('',*,*,#5732,.T.);
#7620=ORIENTED_EDGE('',*,*,#5729,.T.);
#7621=ORIENTED_EDGE('',*,*,#5726,.T.);
#7622=ORIENTED_EDGE('',*,*,#5723,.T.);
#7623=ORIENTED_EDGE('',*,*,#5720,.T.);
#7624=ORIENTED_EDGE('',*,*,#5746,.T.);
#7625=ORIENTED_EDGE('',*,*,#5745,.T.);
#7626=ORIENTED_EDGE('',*,*,#5747,.F.);
#7627=ORIENTED_EDGE('',*,*,#5748,.F.);
#7628=ORIENTED_EDGE('',*,*,#5749,.T.);
#7629=ORIENTED_EDGE('',*,*,#5748,.T.);
#7630=ORIENTED_EDGE('',*,*,#5750,.F.);
#7631=ORIENTED_EDGE('',*,*,#5740,.F.);
#7632=ORIENTED_EDGE('',*,*,#5712,.T.);
#7633=ORIENTED_EDGE('',*,*,#5715,.T.);
#7634=ORIENTED_EDGE('',*,*,#5736,.T.);
#7635=ORIENTED_EDGE('',*,*,#5733,.T.);
#7636=ORIENTED_EDGE('',*,*,#5730,.T.);
#7637=ORIENTED_EDGE('',*,*,#5727,.T.);
#7638=ORIENTED_EDGE('',*,*,#5724,.T.);
#7639=ORIENTED_EDGE('',*,*,#5721,.T.);
#7640=ORIENTED_EDGE('',*,*,#5718,.T.);
#7641=ORIENTED_EDGE('',*,*,#5709,.T.);
#7642=ORIENTED_EDGE('',*,*,#5706,.T.);
#7643=ORIENTED_EDGE('',*,*,#5703,.T.);
#7644=ORIENTED_EDGE('',*,*,#5700,.T.);
#7645=ORIENTED_EDGE('',*,*,#5750,.T.);
#7646=ORIENTED_EDGE('',*,*,#5747,.T.);
#7647=ORIENTED_EDGE('',*,*,#5744,.T.);
#7648=ORIENTED_EDGE('',*,*,#5741,.T.);
#7649=ORIENTED_EDGE('',*,*,#5749,.F.);
#7650=ORIENTED_EDGE('',*,*,#5739,.F.);
#7651=ORIENTED_EDGE('',*,*,#5743,.F.);
#7652=ORIENTED_EDGE('',*,*,#5746,.F.);
#7653=ORIENTED_EDGE('',*,*,#5751,.F.);
#7654=ORIENTED_EDGE('',*,*,#5752,.T.);
#7655=ORIENTED_EDGE('',*,*,#5753,.F.);
#7656=ORIENTED_EDGE('',*,*,#5752,.F.);
#7657=ORIENTED_EDGE('',*,*,#5754,.F.);
#7658=ORIENTED_EDGE('',*,*,#5755,.T.);
#7659=ORIENTED_EDGE('',*,*,#5756,.F.);
#7660=ORIENTED_EDGE('',*,*,#5755,.F.);
#7661=ORIENTED_EDGE('',*,*,#5757,.F.);
#7662=ORIENTED_EDGE('',*,*,#5758,.T.);
#7663=ORIENTED_EDGE('',*,*,#5759,.F.);
#7664=ORIENTED_EDGE('',*,*,#5758,.F.);
#7665=ORIENTED_EDGE('',*,*,#5760,.F.);
#7666=ORIENTED_EDGE('',*,*,#5761,.T.);
#7667=ORIENTED_EDGE('',*,*,#5762,.F.);
#7668=ORIENTED_EDGE('',*,*,#5761,.F.);
#7669=ORIENTED_EDGE('',*,*,#5763,.F.);
#7670=ORIENTED_EDGE('',*,*,#5764,.T.);
#7671=ORIENTED_EDGE('',*,*,#5765,.F.);
#7672=ORIENTED_EDGE('',*,*,#5764,.F.);
#7673=ORIENTED_EDGE('',*,*,#5766,.F.);
#7674=ORIENTED_EDGE('',*,*,#5767,.T.);
#7675=ORIENTED_EDGE('',*,*,#5768,.F.);
#7676=ORIENTED_EDGE('',*,*,#5767,.F.);
#7677=ORIENTED_EDGE('',*,*,#5769,.F.);
#7678=ORIENTED_EDGE('',*,*,#5770,.T.);
#7679=ORIENTED_EDGE('',*,*,#5771,.F.);
#7680=ORIENTED_EDGE('',*,*,#5770,.F.);
#7681=ORIENTED_EDGE('',*,*,#5772,.T.);
#7682=ORIENTED_EDGE('',*,*,#5773,.T.);
#7683=ORIENTED_EDGE('',*,*,#5774,.F.);
#7684=ORIENTED_EDGE('',*,*,#5775,.F.);
#7685=ORIENTED_EDGE('',*,*,#5776,.T.);
#7686=ORIENTED_EDGE('',*,*,#5775,.T.);
#7687=ORIENTED_EDGE('',*,*,#5777,.F.);
#7688=ORIENTED_EDGE('',*,*,#5778,.F.);
#7689=ORIENTED_EDGE('',*,*,#5771,.T.);
#7690=ORIENTED_EDGE('',*,*,#5768,.T.);
#7691=ORIENTED_EDGE('',*,*,#5765,.T.);
#7692=ORIENTED_EDGE('',*,*,#5762,.T.);
#7693=ORIENTED_EDGE('',*,*,#5759,.T.);
#7694=ORIENTED_EDGE('',*,*,#5756,.T.);
#7695=ORIENTED_EDGE('',*,*,#5753,.T.);
#7696=ORIENTED_EDGE('',*,*,#5779,.T.);
#7697=ORIENTED_EDGE('',*,*,#5778,.T.);
#7698=ORIENTED_EDGE('',*,*,#5780,.F.);
#7699=ORIENTED_EDGE('',*,*,#5781,.F.);
#7700=ORIENTED_EDGE('',*,*,#5782,.T.);
#7701=ORIENTED_EDGE('',*,*,#5781,.T.);
#7702=ORIENTED_EDGE('',*,*,#5783,.F.);
#7703=ORIENTED_EDGE('',*,*,#5773,.F.);
#7704=ORIENTED_EDGE('',*,*,#5769,.T.);
#7705=ORIENTED_EDGE('',*,*,#5766,.T.);
#7706=ORIENTED_EDGE('',*,*,#5763,.T.);
#7707=ORIENTED_EDGE('',*,*,#5760,.T.);
#7708=ORIENTED_EDGE('',*,*,#5757,.T.);
#7709=ORIENTED_EDGE('',*,*,#5754,.T.);
#7710=ORIENTED_EDGE('',*,*,#5751,.T.);
#7711=ORIENTED_EDGE('',*,*,#5783,.T.);
#7712=ORIENTED_EDGE('',*,*,#5780,.T.);
#7713=ORIENTED_EDGE('',*,*,#5777,.T.);
#7714=ORIENTED_EDGE('',*,*,#5774,.T.);
#7715=ORIENTED_EDGE('',*,*,#5782,.F.);
#7716=ORIENTED_EDGE('',*,*,#5772,.F.);
#7717=ORIENTED_EDGE('',*,*,#5776,.F.);
#7718=ORIENTED_EDGE('',*,*,#5779,.F.);
#7719=ORIENTED_EDGE('',*,*,#5784,.F.);
#7720=ORIENTED_EDGE('',*,*,#5785,.T.);
#7721=ORIENTED_EDGE('',*,*,#5786,.F.);
#7722=ORIENTED_EDGE('',*,*,#5785,.F.);
#7723=ORIENTED_EDGE('',*,*,#5787,.F.);
#7724=ORIENTED_EDGE('',*,*,#5788,.T.);
#7725=ORIENTED_EDGE('',*,*,#5789,.F.);
#7726=ORIENTED_EDGE('',*,*,#5788,.F.);
#7727=ORIENTED_EDGE('',*,*,#5790,.F.);
#7728=ORIENTED_EDGE('',*,*,#5791,.T.);
#7729=ORIENTED_EDGE('',*,*,#5792,.F.);
#7730=ORIENTED_EDGE('',*,*,#5791,.F.);
#7731=ORIENTED_EDGE('',*,*,#5793,.F.);
#7732=ORIENTED_EDGE('',*,*,#5794,.T.);
#7733=ORIENTED_EDGE('',*,*,#5795,.F.);
#7734=ORIENTED_EDGE('',*,*,#5794,.F.);
#7735=ORIENTED_EDGE('',*,*,#5796,.F.);
#7736=ORIENTED_EDGE('',*,*,#5797,.T.);
#7737=ORIENTED_EDGE('',*,*,#5798,.F.);
#7738=ORIENTED_EDGE('',*,*,#5797,.F.);
#7739=ORIENTED_EDGE('',*,*,#5799,.F.);
#7740=ORIENTED_EDGE('',*,*,#5800,.T.);
#7741=ORIENTED_EDGE('',*,*,#5801,.F.);
#7742=ORIENTED_EDGE('',*,*,#5800,.F.);
#7743=ORIENTED_EDGE('',*,*,#5802,.F.);
#7744=ORIENTED_EDGE('',*,*,#5803,.T.);
#7745=ORIENTED_EDGE('',*,*,#5804,.F.);
#7746=ORIENTED_EDGE('',*,*,#5803,.F.);
#7747=ORIENTED_EDGE('',*,*,#5805,.T.);
#7748=ORIENTED_EDGE('',*,*,#5806,.T.);
#7749=ORIENTED_EDGE('',*,*,#5807,.F.);
#7750=ORIENTED_EDGE('',*,*,#5808,.F.);
#7751=ORIENTED_EDGE('',*,*,#5809,.T.);
#7752=ORIENTED_EDGE('',*,*,#5808,.T.);
#7753=ORIENTED_EDGE('',*,*,#5810,.F.);
#7754=ORIENTED_EDGE('',*,*,#5811,.F.);
#7755=ORIENTED_EDGE('',*,*,#5804,.T.);
#7756=ORIENTED_EDGE('',*,*,#5801,.T.);
#7757=ORIENTED_EDGE('',*,*,#5798,.T.);
#7758=ORIENTED_EDGE('',*,*,#5795,.T.);
#7759=ORIENTED_EDGE('',*,*,#5792,.T.);
#7760=ORIENTED_EDGE('',*,*,#5789,.T.);
#7761=ORIENTED_EDGE('',*,*,#5786,.T.);
#7762=ORIENTED_EDGE('',*,*,#5812,.T.);
#7763=ORIENTED_EDGE('',*,*,#5811,.T.);
#7764=ORIENTED_EDGE('',*,*,#5813,.F.);
#7765=ORIENTED_EDGE('',*,*,#5814,.F.);
#7766=ORIENTED_EDGE('',*,*,#5815,.T.);
#7767=ORIENTED_EDGE('',*,*,#5814,.T.);
#7768=ORIENTED_EDGE('',*,*,#5816,.F.);
#7769=ORIENTED_EDGE('',*,*,#5806,.F.);
#7770=ORIENTED_EDGE('',*,*,#5802,.T.);
#7771=ORIENTED_EDGE('',*,*,#5799,.T.);
#7772=ORIENTED_EDGE('',*,*,#5796,.T.);
#7773=ORIENTED_EDGE('',*,*,#5793,.T.);
#7774=ORIENTED_EDGE('',*,*,#5790,.T.);
#7775=ORIENTED_EDGE('',*,*,#5787,.T.);
#7776=ORIENTED_EDGE('',*,*,#5784,.T.);
#7777=ORIENTED_EDGE('',*,*,#5816,.T.);
#7778=ORIENTED_EDGE('',*,*,#5813,.T.);
#7779=ORIENTED_EDGE('',*,*,#5810,.T.);
#7780=ORIENTED_EDGE('',*,*,#5807,.T.);
#7781=ORIENTED_EDGE('',*,*,#5815,.F.);
#7782=ORIENTED_EDGE('',*,*,#5805,.F.);
#7783=ORIENTED_EDGE('',*,*,#5809,.F.);
#7784=ORIENTED_EDGE('',*,*,#5812,.F.);
#7785=ORIENTED_EDGE('',*,*,#5817,.F.);
#7786=ORIENTED_EDGE('',*,*,#5818,.F.);
#7787=ORIENTED_EDGE('',*,*,#5819,.F.);
#7788=ORIENTED_EDGE('',*,*,#5820,.F.);
#7789=ORIENTED_EDGE('',*,*,#5821,.T.);
#7790=ORIENTED_EDGE('',*,*,#5818,.T.);
#7791=ORIENTED_EDGE('',*,*,#5822,.F.);
#7792=ORIENTED_EDGE('',*,*,#5823,.F.);
#7793=ORIENTED_EDGE('',*,*,#5824,.F.);
#7794=ORIENTED_EDGE('',*,*,#5819,.T.);
#7795=ORIENTED_EDGE('',*,*,#5821,.F.);
#7796=ORIENTED_EDGE('',*,*,#5825,.F.);
#7797=ORIENTED_EDGE('',*,*,#5826,.F.);
#7798=ORIENTED_EDGE('',*,*,#5827,.F.);
#7799=ORIENTED_EDGE('',*,*,#5828,.F.);
#7800=ORIENTED_EDGE('',*,*,#5829,.T.);
#7801=ORIENTED_EDGE('',*,*,#5830,.F.);
#7802=ORIENTED_EDGE('',*,*,#5831,.F.);
#7803=ORIENTED_EDGE('',*,*,#5826,.T.);
#7804=ORIENTED_EDGE('',*,*,#5832,.F.);
#7805=ORIENTED_EDGE('',*,*,#5833,.F.);
#7806=ORIENTED_EDGE('',*,*,#5829,.F.);
#7807=ORIENTED_EDGE('',*,*,#5834,.F.);
#7808=ORIENTED_EDGE('',*,*,#5835,.T.);
#7809=ORIENTED_EDGE('',*,*,#5827,.T.);
#7810=ORIENTED_EDGE('',*,*,#5831,.T.);
#7811=ORIENTED_EDGE('',*,*,#5836,.T.);
#7812=ORIENTED_EDGE('',*,*,#5822,.T.);
#7813=ORIENTED_EDGE('',*,*,#5817,.T.);
#7814=ORIENTED_EDGE('',*,*,#5824,.T.);
#7815=ORIENTED_EDGE('',*,*,#5837,.T.);
#7816=ORIENTED_EDGE('',*,*,#5832,.T.);
#7817=ORIENTED_EDGE('',*,*,#5825,.T.);
#7818=ORIENTED_EDGE('',*,*,#5835,.F.);
#7819=ORIENTED_EDGE('',*,*,#5838,.T.);
#7820=ORIENTED_EDGE('',*,*,#5823,.T.);
#7821=ORIENTED_EDGE('',*,*,#5836,.F.);
#7822=ORIENTED_EDGE('',*,*,#5830,.T.);
#7823=ORIENTED_EDGE('',*,*,#5833,.T.);
#7824=ORIENTED_EDGE('',*,*,#5837,.F.);
#7825=ORIENTED_EDGE('',*,*,#5838,.F.);
#7826=ORIENTED_EDGE('',*,*,#5839,.T.);
#7827=ORIENTED_EDGE('',*,*,#5840,.T.);
#7828=ORIENTED_EDGE('',*,*,#5839,.F.);
#7829=ORIENTED_EDGE('',*,*,#5840,.F.);
#7830=ORIENTED_EDGE('',*,*,#5820,.T.);
#7831=ORIENTED_EDGE('',*,*,#5828,.T.);
#7832=ORIENTED_EDGE('',*,*,#5841,.F.);
#7833=ORIENTED_EDGE('',*,*,#5842,.F.);
#7834=ORIENTED_EDGE('',*,*,#5843,.T.);
#7835=ORIENTED_EDGE('',*,*,#5841,.T.);
#7836=ORIENTED_EDGE('',*,*,#5843,.F.);
#7837=ORIENTED_EDGE('',*,*,#5834,.T.);
#7838=ORIENTED_EDGE('',*,*,#5842,.T.);
#7839=ORIENTED_EDGE('',*,*,#5844,.F.);
#7840=ORIENTED_EDGE('',*,*,#5845,.T.);
#7841=ORIENTED_EDGE('',*,*,#5846,.T.);
#7842=ORIENTED_EDGE('',*,*,#5845,.F.);
#7843=ORIENTED_EDGE('',*,*,#5846,.F.);
#7844=ORIENTED_EDGE('',*,*,#5847,.F.);
#7845=ORIENTED_EDGE('',*,*,#5848,.F.);
#7846=ORIENTED_EDGE('',*,*,#5849,.T.);
#7847=ORIENTED_EDGE('',*,*,#5850,.T.);
#7848=ORIENTED_EDGE('',*,*,#5849,.F.);
#7849=ORIENTED_EDGE('',*,*,#5850,.F.);
#7850=ORIENTED_EDGE('',*,*,#5851,.F.);
#7851=ORIENTED_EDGE('',*,*,#5852,.F.);
#7852=ORIENTED_EDGE('',*,*,#5853,.T.);
#7853=ORIENTED_EDGE('',*,*,#5854,.T.);
#7854=ORIENTED_EDGE('',*,*,#5853,.F.);
#7855=ORIENTED_EDGE('',*,*,#5854,.F.);
#7856=ORIENTED_EDGE('',*,*,#5855,.F.);
#7857=ORIENTED_EDGE('',*,*,#5856,.F.);
#7858=ORIENTED_EDGE('',*,*,#5857,.T.);
#7859=ORIENTED_EDGE('',*,*,#5858,.T.);
#7860=ORIENTED_EDGE('',*,*,#5857,.F.);
#7861=ORIENTED_EDGE('',*,*,#5858,.F.);
#7862=ORIENTED_EDGE('',*,*,#5859,.F.);
#7863=ORIENTED_EDGE('',*,*,#5847,.T.);
#7864=ORIENTED_EDGE('',*,*,#5860,.T.);
#7865=ORIENTED_EDGE('',*,*,#5861,.F.);
#7866=ORIENTED_EDGE('',*,*,#5860,.F.);
#7867=ORIENTED_EDGE('',*,*,#5851,.T.);
#7868=ORIENTED_EDGE('',*,*,#5862,.T.);
#7869=ORIENTED_EDGE('',*,*,#5863,.F.);
#7870=ORIENTED_EDGE('',*,*,#5862,.F.);
#7871=ORIENTED_EDGE('',*,*,#5855,.T.);
#7872=ORIENTED_EDGE('',*,*,#5864,.T.);
#7873=ORIENTED_EDGE('',*,*,#5865,.F.);
#7874=ORIENTED_EDGE('',*,*,#5864,.F.);
#7875=ORIENTED_EDGE('',*,*,#5859,.T.);
#7876=ORIENTED_EDGE('',*,*,#5866,.T.);
#7877=ORIENTED_EDGE('',*,*,#5867,.F.);
#7878=ORIENTED_EDGE('',*,*,#5866,.F.);
#7879=ORIENTED_EDGE('',*,*,#5868,.T.);
#7880=ORIENTED_EDGE('',*,*,#5869,.T.);
#7881=ORIENTED_EDGE('',*,*,#5870,.F.);
#7882=ORIENTED_EDGE('',*,*,#5871,.F.);
#7883=ORIENTED_EDGE('',*,*,#5872,.T.);
#7884=ORIENTED_EDGE('',*,*,#5871,.T.);
#7885=ORIENTED_EDGE('',*,*,#5873,.F.);
#7886=ORIENTED_EDGE('',*,*,#5874,.F.);
#7887=ORIENTED_EDGE('',*,*,#5861,.T.);
#7888=ORIENTED_EDGE('',*,*,#5863,.T.);
#7889=ORIENTED_EDGE('',*,*,#5865,.T.);
#7890=ORIENTED_EDGE('',*,*,#5867,.T.);
#7891=ORIENTED_EDGE('',*,*,#5875,.T.);
#7892=ORIENTED_EDGE('',*,*,#5874,.T.);
#7893=ORIENTED_EDGE('',*,*,#5876,.F.);
#7894=ORIENTED_EDGE('',*,*,#5877,.F.);
#7895=ORIENTED_EDGE('',*,*,#5878,.T.);
#7896=ORIENTED_EDGE('',*,*,#5877,.T.);
#7897=ORIENTED_EDGE('',*,*,#5879,.F.);
#7898=ORIENTED_EDGE('',*,*,#5869,.F.);
#7899=ORIENTED_EDGE('',*,*,#5856,.T.);
#7900=ORIENTED_EDGE('',*,*,#5852,.T.);
#7901=ORIENTED_EDGE('',*,*,#5848,.T.);
#7902=ORIENTED_EDGE('',*,*,#5844,.T.);
#7903=ORIENTED_EDGE('',*,*,#5879,.T.);
#7904=ORIENTED_EDGE('',*,*,#5876,.T.);
#7905=ORIENTED_EDGE('',*,*,#5873,.T.);
#7906=ORIENTED_EDGE('',*,*,#5870,.T.);
#7907=ORIENTED_EDGE('',*,*,#5878,.F.);
#7908=ORIENTED_EDGE('',*,*,#5868,.F.);
#7909=ORIENTED_EDGE('',*,*,#5872,.F.);
#7910=ORIENTED_EDGE('',*,*,#5875,.F.);
#7911=ORIENTED_EDGE('',*,*,#5880,.F.);
#7912=ORIENTED_EDGE('',*,*,#5881,.F.);
#7913=ORIENTED_EDGE('',*,*,#5882,.F.);
#7914=ORIENTED_EDGE('',*,*,#5883,.F.);
#7915=ORIENTED_EDGE('',*,*,#5884,.F.);
#7916=ORIENTED_EDGE('',*,*,#5883,.T.);
#7917=ORIENTED_EDGE('',*,*,#5885,.F.);
#7918=ORIENTED_EDGE('',*,*,#5886,.T.);
#7919=ORIENTED_EDGE('',*,*,#5887,.F.);
#7920=ORIENTED_EDGE('',*,*,#5886,.F.);
#7921=ORIENTED_EDGE('',*,*,#5888,.F.);
#7922=ORIENTED_EDGE('',*,*,#5889,.F.);
#7923=ORIENTED_EDGE('',*,*,#5890,.F.);
#7924=ORIENTED_EDGE('',*,*,#5889,.T.);
#7925=ORIENTED_EDGE('',*,*,#5891,.T.);
#7926=ORIENTED_EDGE('',*,*,#5881,.T.);
#7927=ORIENTED_EDGE('',*,*,#5891,.F.);
#7928=ORIENTED_EDGE('',*,*,#5888,.T.);
#7929=ORIENTED_EDGE('',*,*,#5885,.T.);
#7930=ORIENTED_EDGE('',*,*,#5882,.T.);
#7931=ORIENTED_EDGE('',*,*,#5892,.F.);
#7932=ORIENTED_EDGE('',*,*,#5893,.T.);
#7933=ORIENTED_EDGE('',*,*,#5894,.F.);
#7934=ORIENTED_EDGE('',*,*,#5895,.T.);
#7935=ORIENTED_EDGE('',*,*,#5892,.T.);
#7936=ORIENTED_EDGE('',*,*,#5895,.F.);
#7937=ORIENTED_EDGE('',*,*,#5894,.T.);
#7938=ORIENTED_EDGE('',*,*,#5896,.F.);
#7939=ORIENTED_EDGE('',*,*,#5897,.F.);
#7940=ORIENTED_EDGE('',*,*,#5898,.T.);
#7941=ORIENTED_EDGE('',*,*,#5896,.T.);
#7942=ORIENTED_EDGE('',*,*,#5898,.F.);
#7943=ORIENTED_EDGE('',*,*,#5899,.F.);
#7944=ORIENTED_EDGE('',*,*,#5897,.T.);
#7945=ORIENTED_EDGE('',*,*,#5900,.F.);
#7946=ORIENTED_EDGE('',*,*,#5901,.T.);
#7947=ORIENTED_EDGE('',*,*,#5899,.T.);
#7948=ORIENTED_EDGE('',*,*,#5901,.F.);
#7949=ORIENTED_EDGE('',*,*,#5900,.T.);
#7950=ORIENTED_EDGE('',*,*,#5902,.F.);
#7951=ORIENTED_EDGE('',*,*,#5903,.F.);
#7952=ORIENTED_EDGE('',*,*,#5904,.T.);
#7953=ORIENTED_EDGE('',*,*,#5902,.T.);
#7954=ORIENTED_EDGE('',*,*,#5904,.F.);
#7955=ORIENTED_EDGE('',*,*,#5905,.F.);
#7956=ORIENTED_EDGE('',*,*,#5903,.T.);
#7957=ORIENTED_EDGE('',*,*,#5906,.F.);
#7958=ORIENTED_EDGE('',*,*,#5907,.T.);
#7959=ORIENTED_EDGE('',*,*,#5905,.T.);
#7960=ORIENTED_EDGE('',*,*,#5907,.F.);
#7961=ORIENTED_EDGE('',*,*,#5906,.T.);
#7962=ORIENTED_EDGE('',*,*,#5908,.F.);
#7963=ORIENTED_EDGE('',*,*,#5908,.T.);
#7964=ORIENTED_EDGE('',*,*,#5909,.T.);
#7965=ORIENTED_EDGE('',*,*,#5893,.F.);
#7966=ORIENTED_EDGE('',*,*,#5909,.F.);
#7967=ORIENTED_EDGE('',*,*,#5887,.T.);
#7968=ORIENTED_EDGE('',*,*,#5890,.T.);
#7969=ORIENTED_EDGE('',*,*,#5880,.T.);
#7970=ORIENTED_EDGE('',*,*,#5884,.T.);
#7971=ORIENTED_EDGE('',*,*,#5910,.F.);
#7972=ORIENTED_EDGE('',*,*,#5911,.F.);
#7973=ORIENTED_EDGE('',*,*,#5912,.F.);
#7974=ORIENTED_EDGE('',*,*,#5913,.F.);
#7975=ORIENTED_EDGE('',*,*,#5914,.F.);
#7976=ORIENTED_EDGE('',*,*,#5913,.T.);
#7977=ORIENTED_EDGE('',*,*,#5915,.F.);
#7978=ORIENTED_EDGE('',*,*,#5916,.T.);
#7979=ORIENTED_EDGE('',*,*,#5917,.F.);
#7980=ORIENTED_EDGE('',*,*,#5916,.F.);
#7981=ORIENTED_EDGE('',*,*,#5918,.F.);
#7982=ORIENTED_EDGE('',*,*,#5919,.F.);
#7983=ORIENTED_EDGE('',*,*,#5920,.F.);
#7984=ORIENTED_EDGE('',*,*,#5919,.T.);
#7985=ORIENTED_EDGE('',*,*,#5921,.F.);
#7986=ORIENTED_EDGE('',*,*,#5911,.T.);
#7987=ORIENTED_EDGE('',*,*,#5922,.F.);
#7988=ORIENTED_EDGE('',*,*,#5923,.T.);
#7989=ORIENTED_EDGE('',*,*,#5924,.F.);
#7990=ORIENTED_EDGE('',*,*,#5925,.T.);
#7991=ORIENTED_EDGE('',*,*,#5922,.T.);
#7992=ORIENTED_EDGE('',*,*,#5925,.F.);
#7993=ORIENTED_EDGE('',*,*,#5917,.T.);
#7994=ORIENTED_EDGE('',*,*,#5920,.T.);
#7995=ORIENTED_EDGE('',*,*,#5910,.T.);
#7996=ORIENTED_EDGE('',*,*,#5914,.T.);
#7997=ORIENTED_EDGE('',*,*,#5924,.T.);
#7998=ORIENTED_EDGE('',*,*,#5926,.F.);
#7999=ORIENTED_EDGE('',*,*,#5926,.T.);
#8000=ORIENTED_EDGE('',*,*,#5927,.T.);
#8001=ORIENTED_EDGE('',*,*,#5923,.F.);
#8002=ORIENTED_EDGE('',*,*,#5927,.F.);
#8003=ORIENTED_EDGE('',*,*,#5918,.T.);
#8004=ORIENTED_EDGE('',*,*,#5915,.T.);
#8005=ORIENTED_EDGE('',*,*,#5912,.T.);
#8006=ORIENTED_EDGE('',*,*,#5921,.T.);
#8007=ORIENTED_EDGE('',*,*,#5928,.T.);
#8008=ORIENTED_EDGE('',*,*,#5929,.T.);
#8009=ORIENTED_EDGE('',*,*,#5930,.T.);
#8010=ORIENTED_EDGE('',*,*,#5931,.F.);
#8011=ORIENTED_EDGE('',*,*,#5932,.T.);
#8012=ORIENTED_EDGE('',*,*,#5933,.T.);
#8013=ORIENTED_EDGE('',*,*,#5934,.T.);
#8014=ORIENTED_EDGE('',*,*,#5929,.F.);
#8015=ORIENTED_EDGE('',*,*,#5935,.T.);
#8016=ORIENTED_EDGE('',*,*,#5936,.T.);
#8017=ORIENTED_EDGE('',*,*,#5937,.T.);
#8018=ORIENTED_EDGE('',*,*,#5933,.F.);
#8019=ORIENTED_EDGE('',*,*,#5938,.T.);
#8020=ORIENTED_EDGE('',*,*,#5939,.T.);
#8021=ORIENTED_EDGE('',*,*,#5940,.T.);
#8022=ORIENTED_EDGE('',*,*,#5936,.F.);
#8023=ORIENTED_EDGE('',*,*,#5941,.T.);
#8024=ORIENTED_EDGE('',*,*,#5942,.T.);
#8025=ORIENTED_EDGE('',*,*,#5943,.T.);
#8026=ORIENTED_EDGE('',*,*,#5939,.F.);
#8027=ORIENTED_EDGE('',*,*,#5944,.T.);
#8028=ORIENTED_EDGE('',*,*,#5931,.T.);
#8029=ORIENTED_EDGE('',*,*,#5945,.T.);
#8030=ORIENTED_EDGE('',*,*,#5942,.F.);
#8031=ORIENTED_EDGE('',*,*,#5944,.F.);
#8032=ORIENTED_EDGE('',*,*,#5941,.F.);
#8033=ORIENTED_EDGE('',*,*,#5938,.F.);
#8034=ORIENTED_EDGE('',*,*,#5935,.F.);
#8035=ORIENTED_EDGE('',*,*,#5932,.F.);
#8036=ORIENTED_EDGE('',*,*,#5928,.F.);
#8037=ORIENTED_EDGE('',*,*,#5945,.F.);
#8038=ORIENTED_EDGE('',*,*,#5930,.F.);
#8039=ORIENTED_EDGE('',*,*,#5934,.F.);
#8040=ORIENTED_EDGE('',*,*,#5937,.F.);
#8041=ORIENTED_EDGE('',*,*,#5940,.F.);
#8042=ORIENTED_EDGE('',*,*,#5943,.F.);
#8043=ORIENTED_EDGE('',*,*,#5946,.F.);
#8044=ORIENTED_EDGE('',*,*,#5947,.F.);
#8045=ORIENTED_EDGE('',*,*,#5948,.F.);
#8046=ORIENTED_EDGE('',*,*,#5949,.T.);
#8047=ORIENTED_EDGE('',*,*,#5947,.T.);
#8048=ORIENTED_EDGE('',*,*,#5949,.F.);
#8049=ORIENTED_EDGE('',*,*,#5950,.F.);
#8050=ORIENTED_EDGE('',*,*,#5951,.T.);
#8051=ORIENTED_EDGE('',*,*,#5948,.T.);
#8052=ORIENTED_EDGE('',*,*,#5951,.F.);
#8053=ORIENTED_EDGE('',*,*,#5952,.F.);
#8054=ORIENTED_EDGE('',*,*,#5953,.T.);
#8055=ORIENTED_EDGE('',*,*,#5950,.T.);
#8056=ORIENTED_EDGE('',*,*,#5953,.F.);
#8057=ORIENTED_EDGE('',*,*,#5952,.T.);
#8058=ORIENTED_EDGE('',*,*,#5954,.F.);
#8059=ORIENTED_EDGE('',*,*,#5955,.F.);
#8060=ORIENTED_EDGE('',*,*,#5956,.T.);
#8061=ORIENTED_EDGE('',*,*,#5954,.T.);
#8062=ORIENTED_EDGE('',*,*,#5956,.F.);
#8063=ORIENTED_EDGE('',*,*,#5946,.T.);
#8064=ORIENTED_EDGE('',*,*,#5957,.T.);
#8065=ORIENTED_EDGE('',*,*,#5955,.T.);
#8066=ORIENTED_EDGE('',*,*,#5957,.F.);
#8067=ORIENTED_EDGE('',*,*,#5958,.F.);
#8068=ORIENTED_EDGE('',*,*,#5959,.T.);
#8069=ORIENTED_EDGE('',*,*,#5960,.F.);
#8070=ORIENTED_EDGE('',*,*,#5959,.F.);
#8071=ORIENTED_EDGE('',*,*,#5958,.T.);
#8072=ORIENTED_EDGE('',*,*,#5961,.F.);
#8073=ORIENTED_EDGE('',*,*,#5962,.T.);
#8074=ORIENTED_EDGE('',*,*,#5963,.T.);
#8075=ORIENTED_EDGE('',*,*,#5962,.F.);
#8076=ORIENTED_EDGE('',*,*,#5963,.F.);
#8077=ORIENTED_EDGE('',*,*,#5964,.T.);
#8078=ORIENTED_EDGE('',*,*,#5965,.F.);
#8079=ORIENTED_EDGE('',*,*,#5966,.F.);
#8080=ORIENTED_EDGE('',*,*,#5967,.F.);
#8081=ORIENTED_EDGE('',*,*,#5964,.F.);
#8082=ORIENTED_EDGE('',*,*,#5968,.T.);
#8083=ORIENTED_EDGE('',*,*,#5966,.T.);
#8084=ORIENTED_EDGE('',*,*,#5968,.F.);
#8085=ORIENTED_EDGE('',*,*,#5967,.T.);
#8086=ORIENTED_EDGE('',*,*,#5969,.T.);
#8087=ORIENTED_EDGE('',*,*,#5970,.T.);
#8088=ORIENTED_EDGE('',*,*,#5969,.F.);
#8089=ORIENTED_EDGE('',*,*,#5971,.T.);
#8090=ORIENTED_EDGE('',*,*,#5970,.F.);
#8091=ORIENTED_EDGE('',*,*,#5972,.F.);
#8092=ORIENTED_EDGE('',*,*,#5973,.F.);
#8093=ORIENTED_EDGE('',*,*,#5971,.F.);
#8094=ORIENTED_EDGE('',*,*,#5974,.T.);
#8095=ORIENTED_EDGE('',*,*,#5972,.T.);
#8096=ORIENTED_EDGE('',*,*,#5974,.F.);
#8097=ORIENTED_EDGE('',*,*,#5973,.T.);
#8098=ORIENTED_EDGE('',*,*,#5975,.T.);
#8099=ORIENTED_EDGE('',*,*,#5976,.T.);
#8100=ORIENTED_EDGE('',*,*,#5975,.F.);
#8101=ORIENTED_EDGE('',*,*,#5977,.F.);
#8102=ORIENTED_EDGE('',*,*,#5978,.T.);
#8103=ORIENTED_EDGE('',*,*,#5965,.T.);
#8104=ORIENTED_EDGE('',*,*,#5978,.F.);
#8105=ORIENTED_EDGE('',*,*,#5977,.T.);
#8106=ORIENTED_EDGE('',*,*,#5960,.T.);
#8107=ORIENTED_EDGE('',*,*,#5976,.F.);
#8108=ORIENTED_EDGE('',*,*,#5961,.T.);
#8109=ORIENTED_EDGE('',*,*,#5979,.F.);
#8110=ORIENTED_EDGE('',*,*,#5980,.T.);
#8111=ORIENTED_EDGE('',*,*,#5981,.T.);
#8112=ORIENTED_EDGE('',*,*,#5980,.F.);
#8113=ORIENTED_EDGE('',*,*,#5982,.F.);
#8114=ORIENTED_EDGE('',*,*,#5983,.T.);
#8115=ORIENTED_EDGE('',*,*,#5984,.T.);
#8116=ORIENTED_EDGE('',*,*,#5983,.F.);
#8117=ORIENTED_EDGE('',*,*,#5982,.T.);
#8118=ORIENTED_EDGE('',*,*,#5979,.T.);
#8119=ORIENTED_EDGE('',*,*,#5984,.F.);
#8120=ORIENTED_EDGE('',*,*,#5981,.F.);
#8121=ORIENTED_EDGE('',*,*,#5985,.F.);
#8122=ORIENTED_EDGE('',*,*,#5986,.T.);
#8123=ORIENTED_EDGE('',*,*,#5987,.T.);
#8124=ORIENTED_EDGE('',*,*,#5986,.F.);
#8125=ORIENTED_EDGE('',*,*,#5988,.F.);
#8126=ORIENTED_EDGE('',*,*,#5989,.T.);
#8127=ORIENTED_EDGE('',*,*,#5990,.T.);
#8128=ORIENTED_EDGE('',*,*,#5989,.F.);
#8129=ORIENTED_EDGE('',*,*,#5988,.T.);
#8130=ORIENTED_EDGE('',*,*,#5985,.T.);
#8131=ORIENTED_EDGE('',*,*,#5990,.F.);
#8132=ORIENTED_EDGE('',*,*,#5987,.F.);
#8133=ORIENTED_EDGE('',*,*,#5991,.F.);
#8134=ORIENTED_EDGE('',*,*,#5992,.T.);
#8135=ORIENTED_EDGE('',*,*,#5993,.F.);
#8136=ORIENTED_EDGE('',*,*,#5992,.F.);
#8137=ORIENTED_EDGE('',*,*,#5994,.F.);
#8138=ORIENTED_EDGE('',*,*,#5995,.T.);
#8139=ORIENTED_EDGE('',*,*,#5996,.F.);
#8140=ORIENTED_EDGE('',*,*,#5997,.F.);
#8141=ORIENTED_EDGE('',*,*,#5998,.F.);
#8142=ORIENTED_EDGE('',*,*,#5999,.F.);
#8143=ORIENTED_EDGE('',*,*,#5995,.F.);
#8144=ORIENTED_EDGE('',*,*,#6000,.F.);
#8145=ORIENTED_EDGE('',*,*,#6001,.T.);
#8146=ORIENTED_EDGE('',*,*,#6002,.F.);
#8147=ORIENTED_EDGE('',*,*,#6003,.F.);
#8148=ORIENTED_EDGE('',*,*,#6004,.F.);
#8149=ORIENTED_EDGE('',*,*,#6001,.F.);
#8150=ORIENTED_EDGE('',*,*,#6005,.F.);
#8151=ORIENTED_EDGE('',*,*,#5997,.T.);
#8152=ORIENTED_EDGE('',*,*,#5993,.T.);
#8153=ORIENTED_EDGE('',*,*,#6006,.F.);
#8154=ORIENTED_EDGE('',*,*,#6007,.F.);
#8155=ORIENTED_EDGE('',*,*,#6008,.T.);
#8156=ORIENTED_EDGE('',*,*,#5998,.T.);
#8157=ORIENTED_EDGE('',*,*,#6005,.T.);
#8158=ORIENTED_EDGE('',*,*,#5996,.T.);
#8159=ORIENTED_EDGE('',*,*,#6009,.T.);
#8160=ORIENTED_EDGE('',*,*,#6010,.T.);
#8161=ORIENTED_EDGE('',*,*,#6009,.F.);
#8162=ORIENTED_EDGE('',*,*,#6000,.T.);
#8163=ORIENTED_EDGE('',*,*,#5994,.T.);
#8164=ORIENTED_EDGE('',*,*,#5999,.T.);
#8165=ORIENTED_EDGE('',*,*,#6008,.F.);
#8166=ORIENTED_EDGE('',*,*,#6011,.F.);
#8167=ORIENTED_EDGE('',*,*,#6012,.T.);
#8168=ORIENTED_EDGE('',*,*,#6003,.T.);
#8169=ORIENTED_EDGE('',*,*,#6002,.T.);
#8170=ORIENTED_EDGE('',*,*,#6013,.T.);
#8171=ORIENTED_EDGE('',*,*,#6006,.T.);
#8172=ORIENTED_EDGE('',*,*,#6013,.F.);
#8173=ORIENTED_EDGE('',*,*,#6004,.T.);
#8174=ORIENTED_EDGE('',*,*,#6012,.F.);
#8175=ORIENTED_EDGE('',*,*,#6011,.T.);
#8176=ORIENTED_EDGE('',*,*,#6007,.T.);
#8177=ORIENTED_EDGE('',*,*,#5991,.T.);
#8178=ORIENTED_EDGE('',*,*,#6010,.F.);
#8179=ORIENTED_EDGE('',*,*,#6014,.F.);
#8180=ORIENTED_EDGE('',*,*,#6015,.T.);
#8181=ORIENTED_EDGE('',*,*,#6016,.T.);
#8182=ORIENTED_EDGE('',*,*,#6015,.F.);
#8183=ORIENTED_EDGE('',*,*,#6017,.F.);
#8184=ORIENTED_EDGE('',*,*,#6018,.T.);
#8185=ORIENTED_EDGE('',*,*,#6019,.T.);
#8186=ORIENTED_EDGE('',*,*,#6018,.F.);
#8187=ORIENTED_EDGE('',*,*,#6017,.T.);
#8188=ORIENTED_EDGE('',*,*,#6014,.T.);
#8189=ORIENTED_EDGE('',*,*,#6019,.F.);
#8190=ORIENTED_EDGE('',*,*,#6016,.F.);
#8191=ORIENTED_EDGE('',*,*,#6020,.F.);
#8192=ORIENTED_EDGE('',*,*,#6021,.T.);
#8193=ORIENTED_EDGE('',*,*,#6022,.T.);
#8194=ORIENTED_EDGE('',*,*,#6021,.F.);
#8195=ORIENTED_EDGE('',*,*,#6023,.F.);
#8196=ORIENTED_EDGE('',*,*,#6024,.T.);
#8197=ORIENTED_EDGE('',*,*,#6025,.T.);
#8198=ORIENTED_EDGE('',*,*,#6024,.F.);
#8199=ORIENTED_EDGE('',*,*,#6023,.T.);
#8200=ORIENTED_EDGE('',*,*,#6020,.T.);
#8201=ORIENTED_EDGE('',*,*,#6025,.F.);
#8202=ORIENTED_EDGE('',*,*,#6022,.F.);
#8203=ORIENTED_EDGE('',*,*,#6026,.F.);
#8204=ORIENTED_EDGE('',*,*,#6027,.T.);
#8205=ORIENTED_EDGE('',*,*,#6028,.F.);
#8206=ORIENTED_EDGE('',*,*,#6029,.F.);
#8207=ORIENTED_EDGE('',*,*,#6030,.F.);
#8208=ORIENTED_EDGE('',*,*,#6031,.F.);
#8209=ORIENTED_EDGE('',*,*,#6027,.F.);
#8210=ORIENTED_EDGE('',*,*,#6032,.F.);
#8211=ORIENTED_EDGE('',*,*,#6033,.T.);
#8212=ORIENTED_EDGE('',*,*,#6034,.F.);
#8213=ORIENTED_EDGE('',*,*,#6035,.F.);
#8214=ORIENTED_EDGE('',*,*,#6036,.F.);
#8215=ORIENTED_EDGE('',*,*,#6033,.F.);
#8216=ORIENTED_EDGE('',*,*,#6037,.F.);
#8217=ORIENTED_EDGE('',*,*,#6029,.T.);
#8218=ORIENTED_EDGE('',*,*,#6038,.F.);
#8219=ORIENTED_EDGE('',*,*,#6039,.T.);
#8220=ORIENTED_EDGE('',*,*,#6030,.T.);
#8221=ORIENTED_EDGE('',*,*,#6037,.T.);
#8222=ORIENTED_EDGE('',*,*,#6028,.T.);
#8223=ORIENTED_EDGE('',*,*,#6040,.T.);
#8224=ORIENTED_EDGE('',*,*,#6041,.T.);
#8225=ORIENTED_EDGE('',*,*,#6040,.F.);
#8226=ORIENTED_EDGE('',*,*,#6032,.T.);
#8227=ORIENTED_EDGE('',*,*,#6026,.T.);
#8228=ORIENTED_EDGE('',*,*,#6031,.T.);
#8229=ORIENTED_EDGE('',*,*,#6039,.F.);
#8230=ORIENTED_EDGE('',*,*,#6042,.F.);
#8231=ORIENTED_EDGE('',*,*,#6043,.T.);
#8232=ORIENTED_EDGE('',*,*,#6035,.T.);
#8233=ORIENTED_EDGE('',*,*,#6034,.T.);
#8234=ORIENTED_EDGE('',*,*,#6044,.T.);
#8235=ORIENTED_EDGE('',*,*,#6045,.T.);
#8236=ORIENTED_EDGE('',*,*,#6044,.F.);
#8237=ORIENTED_EDGE('',*,*,#6036,.T.);
#8238=ORIENTED_EDGE('',*,*,#6043,.F.);
#8239=ORIENTED_EDGE('',*,*,#6042,.T.);
#8240=ORIENTED_EDGE('',*,*,#6038,.T.);
#8241=ORIENTED_EDGE('',*,*,#6045,.F.);
#8242=ORIENTED_EDGE('',*,*,#6041,.F.);
#8243=ORIENTED_EDGE('',*,*,#6046,.F.);
#8244=ORIENTED_EDGE('',*,*,#6047,.F.);
#8245=ORIENTED_EDGE('',*,*,#6048,.T.);
#8246=ORIENTED_EDGE('',*,*,#6046,.T.);
#8247=ORIENTED_EDGE('',*,*,#6048,.F.);
#8248=ORIENTED_EDGE('',*,*,#6049,.F.);
#8249=ORIENTED_EDGE('',*,*,#6050,.T.);
#8250=ORIENTED_EDGE('',*,*,#6047,.T.);
#8251=ORIENTED_EDGE('',*,*,#6050,.F.);
#8252=ORIENTED_EDGE('',*,*,#6051,.F.);
#8253=ORIENTED_EDGE('',*,*,#6052,.T.);
#8254=ORIENTED_EDGE('',*,*,#6049,.T.);
#8255=ORIENTED_EDGE('',*,*,#6052,.F.);
#8256=ORIENTED_EDGE('',*,*,#6051,.T.);
#8257=ORIENTED_EDGE('',*,*,#6053,.F.);
#8258=ORIENTED_EDGE('',*,*,#6054,.F.);
#8259=ORIENTED_EDGE('',*,*,#6055,.T.);
#8260=ORIENTED_EDGE('',*,*,#6053,.T.);
#8261=ORIENTED_EDGE('',*,*,#6055,.F.);
#8262=ORIENTED_EDGE('',*,*,#6056,.F.);
#8263=ORIENTED_EDGE('',*,*,#6057,.T.);
#8264=ORIENTED_EDGE('',*,*,#6054,.T.);
#8265=ORIENTED_EDGE('',*,*,#6057,.F.);
#8266=ORIENTED_EDGE('',*,*,#6058,.F.);
#8267=ORIENTED_EDGE('',*,*,#6059,.T.);
#8268=ORIENTED_EDGE('',*,*,#6056,.T.);
#8269=ORIENTED_EDGE('',*,*,#6059,.F.);
#8270=ORIENTED_EDGE('',*,*,#6058,.T.);
#8271=ORIENTED_EDGE('',*,*,#6060,.T.);
#8272=ORIENTED_EDGE('',*,*,#6061,.T.);
#8273=ORIENTED_EDGE('',*,*,#6062,.T.);
#8274=ORIENTED_EDGE('',*,*,#6063,.F.);
#8275=ORIENTED_EDGE('',*,*,#6064,.T.);
#8276=ORIENTED_EDGE('',*,*,#6065,.T.);
#8277=ORIENTED_EDGE('',*,*,#6066,.T.);
#8278=ORIENTED_EDGE('',*,*,#6061,.F.);
#8279=ORIENTED_EDGE('',*,*,#6067,.T.);
#8280=ORIENTED_EDGE('',*,*,#6068,.T.);
#8281=ORIENTED_EDGE('',*,*,#6069,.T.);
#8282=ORIENTED_EDGE('',*,*,#6065,.F.);
#8283=ORIENTED_EDGE('',*,*,#6070,.T.);
#8284=ORIENTED_EDGE('',*,*,#6071,.T.);
#8285=ORIENTED_EDGE('',*,*,#6072,.T.);
#8286=ORIENTED_EDGE('',*,*,#6068,.F.);
#8287=ORIENTED_EDGE('',*,*,#6073,.T.);
#8288=ORIENTED_EDGE('',*,*,#6074,.T.);
#8289=ORIENTED_EDGE('',*,*,#6075,.T.);
#8290=ORIENTED_EDGE('',*,*,#6071,.F.);
#8291=ORIENTED_EDGE('',*,*,#6076,.T.);
#8292=ORIENTED_EDGE('',*,*,#6063,.T.);
#8293=ORIENTED_EDGE('',*,*,#6077,.T.);
#8294=ORIENTED_EDGE('',*,*,#6074,.F.);
#8295=ORIENTED_EDGE('',*,*,#6076,.F.);
#8296=ORIENTED_EDGE('',*,*,#6073,.F.);
#8297=ORIENTED_EDGE('',*,*,#6070,.F.);
#8298=ORIENTED_EDGE('',*,*,#6067,.F.);
#8299=ORIENTED_EDGE('',*,*,#6064,.F.);
#8300=ORIENTED_EDGE('',*,*,#6060,.F.);
#8301=ORIENTED_EDGE('',*,*,#6077,.F.);
#8302=ORIENTED_EDGE('',*,*,#6062,.F.);
#8303=ORIENTED_EDGE('',*,*,#6066,.F.);
#8304=ORIENTED_EDGE('',*,*,#6069,.F.);
#8305=ORIENTED_EDGE('',*,*,#6072,.F.);
#8306=ORIENTED_EDGE('',*,*,#6075,.F.);
#8307=ORIENTED_EDGE('',*,*,#6078,.F.);
#8308=ORIENTED_EDGE('',*,*,#6079,.T.);
#8309=ORIENTED_EDGE('',*,*,#6080,.T.);
#8310=ORIENTED_EDGE('',*,*,#6081,.F.);
#8311=ORIENTED_EDGE('',*,*,#6082,.F.);
#8312=ORIENTED_EDGE('',*,*,#6083,.T.);
#8313=ORIENTED_EDGE('',*,*,#6084,.T.);
#8314=ORIENTED_EDGE('',*,*,#6079,.F.);
#8315=ORIENTED_EDGE('',*,*,#6085,.F.);
#8316=ORIENTED_EDGE('',*,*,#6086,.T.);
#8317=ORIENTED_EDGE('',*,*,#6087,.T.);
#8318=ORIENTED_EDGE('',*,*,#6083,.F.);
#8319=ORIENTED_EDGE('',*,*,#6088,.F.);
#8320=ORIENTED_EDGE('',*,*,#6089,.T.);
#8321=ORIENTED_EDGE('',*,*,#6090,.T.);
#8322=ORIENTED_EDGE('',*,*,#6086,.F.);
#8323=ORIENTED_EDGE('',*,*,#6091,.F.);
#8324=ORIENTED_EDGE('',*,*,#6092,.T.);
#8325=ORIENTED_EDGE('',*,*,#6093,.T.);
#8326=ORIENTED_EDGE('',*,*,#6089,.F.);
#8327=ORIENTED_EDGE('',*,*,#6094,.F.);
#8328=ORIENTED_EDGE('',*,*,#6081,.T.);
#8329=ORIENTED_EDGE('',*,*,#6095,.T.);
#8330=ORIENTED_EDGE('',*,*,#6092,.F.);
#8331=ORIENTED_EDGE('',*,*,#6095,.F.);
#8332=ORIENTED_EDGE('',*,*,#6080,.F.);
#8333=ORIENTED_EDGE('',*,*,#6084,.F.);
#8334=ORIENTED_EDGE('',*,*,#6087,.F.);
#8335=ORIENTED_EDGE('',*,*,#6090,.F.);
#8336=ORIENTED_EDGE('',*,*,#6093,.F.);
#8337=ORIENTED_EDGE('',*,*,#6096,.F.);
#8338=ORIENTED_EDGE('',*,*,#6078,.T.);
#8339=ORIENTED_EDGE('',*,*,#6094,.T.);
#8340=ORIENTED_EDGE('',*,*,#6091,.T.);
#8341=ORIENTED_EDGE('',*,*,#6088,.T.);
#8342=ORIENTED_EDGE('',*,*,#6085,.T.);
#8343=ORIENTED_EDGE('',*,*,#6082,.T.);
#8344=ORIENTED_EDGE('',*,*,#6097,.F.);
#8345=ORIENTED_EDGE('',*,*,#6098,.T.);
#8346=ORIENTED_EDGE('',*,*,#6096,.T.);
#8347=ORIENTED_EDGE('',*,*,#6098,.F.);
#8348=ORIENTED_EDGE('',*,*,#6099,.F.);
#8349=ORIENTED_EDGE('',*,*,#6100,.T.);
#8350=ORIENTED_EDGE('',*,*,#6097,.T.);
#8351=ORIENTED_EDGE('',*,*,#6100,.F.);
#8352=ORIENTED_EDGE('',*,*,#6101,.F.);
#8353=ORIENTED_EDGE('',*,*,#6102,.T.);
#8354=ORIENTED_EDGE('',*,*,#6099,.T.);
#8355=ORIENTED_EDGE('',*,*,#6102,.F.);
#8356=ORIENTED_EDGE('',*,*,#6101,.T.);
#8357=CYLINDRICAL_SURFACE('',#9580,0.164999999999999);
#8358=CYLINDRICAL_SURFACE('',#9583,0.164999999999999);
#8359=CYLINDRICAL_SURFACE('',#9586,0.164999999999999);
#8360=CYLINDRICAL_SURFACE('',#9589,0.164999999999999);
#8361=CYLINDRICAL_SURFACE('',#9592,0.164999999999999);
#8362=CYLINDRICAL_SURFACE('',#9595,0.164999999999999);
#8363=CYLINDRICAL_SURFACE('',#9598,0.164999999999999);
#8364=CYLINDRICAL_SURFACE('',#9601,0.164999999999999);
#8365=CYLINDRICAL_SURFACE('',#9604,0.164999999999999);
#8366=CYLINDRICAL_SURFACE('',#9607,0.164999999999999);
#8367=CYLINDRICAL_SURFACE('',#9610,0.164999999999999);
#8368=CYLINDRICAL_SURFACE('',#9613,0.164999999999999);
#8369=CYLINDRICAL_SURFACE('',#9637,0.4);
#8370=CYLINDRICAL_SURFACE('',#9640,0.4);
#8371=CYLINDRICAL_SURFACE('',#9645,0.164999999999999);
#8372=CYLINDRICAL_SURFACE('',#9649,0.4);
#8373=CYLINDRICAL_SURFACE('',#9654,0.4);
#8374=CYLINDRICAL_SURFACE('',#9660,0.225);
#8375=CYLINDRICAL_SURFACE('',#9662,0.225);
#8376=CYLINDRICAL_SURFACE('',#9664,0.6);
#8377=CYLINDRICAL_SURFACE('',#9673,0.4);
#8378=CYLINDRICAL_SURFACE('',#9676,0.4);
#8379=CYLINDRICAL_SURFACE('',#9681,0.164999999999999);
#8380=CYLINDRICAL_SURFACE('',#9685,0.4);
#8381=CYLINDRICAL_SURFACE('',#9690,0.4);
#8382=CYLINDRICAL_SURFACE('',#9696,0.225);
#8383=CYLINDRICAL_SURFACE('',#9698,0.225);
#8384=CYLINDRICAL_SURFACE('',#9700,0.6);
#8385=CYLINDRICAL_SURFACE('',#9709,0.4);
#8386=CYLINDRICAL_SURFACE('',#9712,0.4);
#8387=CYLINDRICAL_SURFACE('',#9717,0.164999999999999);
#8388=CYLINDRICAL_SURFACE('',#9721,0.4);
#8389=CYLINDRICAL_SURFACE('',#9726,0.4);
#8390=CYLINDRICAL_SURFACE('',#9732,0.225);
#8391=CYLINDRICAL_SURFACE('',#9734,0.225);
#8392=CYLINDRICAL_SURFACE('',#9736,0.6);
#8393=CYLINDRICAL_SURFACE('',#9745,0.4);
#8394=CYLINDRICAL_SURFACE('',#9748,0.4);
#8395=CYLINDRICAL_SURFACE('',#9753,0.164999999999999);
#8396=CYLINDRICAL_SURFACE('',#9757,0.4);
#8397=CYLINDRICAL_SURFACE('',#9762,0.4);
#8398=CYLINDRICAL_SURFACE('',#9768,0.225);
#8399=CYLINDRICAL_SURFACE('',#9770,0.225);
#8400=CYLINDRICAL_SURFACE('',#9772,0.6);
#8401=CYLINDRICAL_SURFACE('',#9781,0.165);
#8402=CYLINDRICAL_SURFACE('',#9784,0.165);
#8403=CYLINDRICAL_SURFACE('',#9787,0.165);
#8404=CYLINDRICAL_SURFACE('',#9790,0.165);
#8405=CYLINDRICAL_SURFACE('',#9793,0.225);
#8406=CYLINDRICAL_SURFACE('',#9796,0.225);
#8407=CYLINDRICAL_SURFACE('',#9799,1.6);
#8408=CYLINDRICAL_SURFACE('',#9813,0.225);
#8409=CYLINDRICAL_SURFACE('',#9816,0.225);
#8410=CYLINDRICAL_SURFACE('',#9819,0.225);
#8411=CYLINDRICAL_SURFACE('',#9822,0.225);
#8412=CYLINDRICAL_SURFACE('',#9825,1.59);
#8413=CYLINDRICAL_SURFACE('',#9830,1.005);
#8414=CYLINDRICAL_SURFACE('',#9832,2.4);
#8415=CYLINDRICAL_SURFACE('',#9838,0.225);
#8416=CYLINDRICAL_SURFACE('',#9841,0.225);
#8417=CYLINDRICAL_SURFACE('',#9844,0.225);
#8418=CYLINDRICAL_SURFACE('',#9847,0.225);
#8419=CYLINDRICAL_SURFACE('',#9850,1.59);
#8420=CYLINDRICAL_SURFACE('',#9855,1.005);
#8421=CYLINDRICAL_SURFACE('',#9857,2.4);
#8422=CYLINDRICAL_SURFACE('',#9863,0.165);
#8423=CYLINDRICAL_SURFACE('',#9866,0.165);
#8424=CYLINDRICAL_SURFACE('',#9869,0.165);
#8425=CYLINDRICAL_SURFACE('',#9872,0.165);
#8426=CYLINDRICAL_SURFACE('',#9875,0.225);
#8427=CYLINDRICAL_SURFACE('',#9878,0.225);
#8428=CYLINDRICAL_SURFACE('',#9881,1.6);
#8429=CYLINDRICAL_SURFACE('',#9895,0.225);
#8430=CYLINDRICAL_SURFACE('',#9898,0.225);
#8431=CYLINDRICAL_SURFACE('',#9901,0.225);
#8432=CYLINDRICAL_SURFACE('',#9904,0.225);
#8433=CYLINDRICAL_SURFACE('',#9907,1.59);
#8434=CYLINDRICAL_SURFACE('',#9912,1.005);
#8435=CYLINDRICAL_SURFACE('',#9914,2.4);
#8436=CYLINDRICAL_SURFACE('',#9920,0.225);
#8437=CYLINDRICAL_SURFACE('',#9923,0.225);
#8438=CYLINDRICAL_SURFACE('',#9926,0.225);
#8439=CYLINDRICAL_SURFACE('',#9929,0.225);
#8440=CYLINDRICAL_SURFACE('',#9932,1.59);
#8441=CYLINDRICAL_SURFACE('',#9937,1.005);
#8442=CYLINDRICAL_SURFACE('',#9939,2.4);
#8443=CYLINDRICAL_SURFACE('',#9948,0.6);
#8444=CYLINDRICAL_SURFACE('',#9962,1.070235);
#8445=CYLINDRICAL_SURFACE('',#9964,0.6);
#8446=CYLINDRICAL_SURFACE('',#9970,1.070235);
#8447=CYLINDRICAL_SURFACE('',#9982,1.129765);
#8448=CYLINDRICAL_SURFACE('',#9989,1.6);
#8449=CYLINDRICAL_SURFACE('',#9994,1.129765);
#8450=CYLINDRICAL_SURFACE('',#10014,1.123812);
#8451=CYLINDRICAL_SURFACE('',#10050,1.076188);
#8452=CYLINDRICAL_SURFACE('',#10064,1.119765);
#8453=CYLINDRICAL_SURFACE('',#10068,1.085235);
#8454=CYLINDRICAL_SURFACE('',#10072,1.119765);
#8455=CYLINDRICAL_SURFACE('',#10076,1.085235);
#8456=CYLINDRICAL_SURFACE('',#10084,0.165);
#8457=CYLINDRICAL_SURFACE('',#10088,0.164999999999999);
#8458=CYLINDRICAL_SURFACE('',#10092,0.165);
#8459=CYLINDRICAL_SURFACE('',#10096,0.164999999999999);
#8460=CYLINDRICAL_SURFACE('',#10100,0.165);
#8461=CYLINDRICAL_SURFACE('',#10104,0.165);
#8462=CYLINDRICAL_SURFACE('',#10108,0.165);
#8463=CYLINDRICAL_SURFACE('',#10111,0.165);
#8464=CYLINDRICAL_SURFACE('',#10114,0.165);
#8465=CYLINDRICAL_SURFACE('',#10117,0.165);
#8466=CYLINDRICAL_SURFACE('',#10120,1.1);
#8467=CYLINDRICAL_SURFACE('',#10123,1.05);
#8468=CYLINDRICAL_SURFACE('',#10126,1.05);
#8469=CYLINDRICAL_SURFACE('',#10136,0.225);
#8470=CYLINDRICAL_SURFACE('',#10139,0.225);
#8471=CYLINDRICAL_SURFACE('',#10142,0.225);
#8472=CYLINDRICAL_SURFACE('',#10145,0.225);
#8473=CYLINDRICAL_SURFACE('',#10148,1.65);
#8474=CYLINDRICAL_SURFACE('',#10151,0.7);
#8475=CYLINDRICAL_SURFACE('',#10154,0.7);
#8476=CYLINDRICAL_SURFACE('',#10164,0.225);
#8477=CYLINDRICAL_SURFACE('',#10167,0.225);
#8478=CYLINDRICAL_SURFACE('',#10170,0.225);
#8479=CYLINDRICAL_SURFACE('',#10173,0.225);
#8480=CYLINDRICAL_SURFACE('',#10176,1.65);
#8481=CYLINDRICAL_SURFACE('',#10179,0.7);
#8482=CYLINDRICAL_SURFACE('',#10182,0.7);
#8483=CYLINDRICAL_SURFACE('',#10196,0.225);
#8484=CYLINDRICAL_SURFACE('',#10203,0.225);
#8485=CYLINDRICAL_SURFACE('',#10207,1.1);
#8486=CYLINDRICAL_SURFACE('',#10213,1.6);
#8487=CYLINDRICAL_SURFACE('',#10217,0.525);
#8488=CYLINDRICAL_SURFACE('',#10221,0.4);
#8489=CYLINDRICAL_SURFACE('',#10226,0.4);
#8490=CYLINDRICAL_SURFACE('',#10231,0.4);
#8491=CYLINDRICAL_SURFACE('',#10236,0.4);
#8492=CYLINDRICAL_SURFACE('',#10241,0.225);
#8493=CYLINDRICAL_SURFACE('',#10243,0.225);
#8494=CYLINDRICAL_SURFACE('',#10245,0.225);
#8495=CYLINDRICAL_SURFACE('',#10247,0.225);
#8496=CYLINDRICAL_SURFACE('',#10257,0.165);
#8497=CYLINDRICAL_SURFACE('',#10261,0.164999999999999);
#8498=CYLINDRICAL_SURFACE('',#10265,0.165);
#8499=CYLINDRICAL_SURFACE('',#10269,0.164999999999999);
#8500=CYLINDRICAL_SURFACE('',#10273,0.165);
#8501=CYLINDRICAL_SURFACE('',#10277,0.165);
#8502=CYLINDRICAL_SURFACE('',#10281,0.165);
#8503=CYLINDRICAL_SURFACE('',#10284,0.165);
#8504=CYLINDRICAL_SURFACE('',#10287,0.165);
#8505=CYLINDRICAL_SURFACE('',#10290,0.165);
#8506=CYLINDRICAL_SURFACE('',#10293,1.1);
#8507=CYLINDRICAL_SURFACE('',#10296,1.05);
#8508=CYLINDRICAL_SURFACE('',#10299,1.05);
#8509=CYLINDRICAL_SURFACE('',#10309,0.225);
#8510=CYLINDRICAL_SURFACE('',#10312,0.225);
#8511=CYLINDRICAL_SURFACE('',#10315,0.225);
#8512=CYLINDRICAL_SURFACE('',#10318,0.225);
#8513=CYLINDRICAL_SURFACE('',#10321,1.65);
#8514=CYLINDRICAL_SURFACE('',#10324,0.7);
#8515=CYLINDRICAL_SURFACE('',#10327,0.7);
#8516=CYLINDRICAL_SURFACE('',#10337,0.225);
#8517=CYLINDRICAL_SURFACE('',#10340,0.225);
#8518=CYLINDRICAL_SURFACE('',#10343,0.225);
#8519=CYLINDRICAL_SURFACE('',#10346,0.225);
#8520=CYLINDRICAL_SURFACE('',#10349,1.65);
#8521=CYLINDRICAL_SURFACE('',#10352,0.7);
#8522=CYLINDRICAL_SURFACE('',#10355,0.7);
#8523=CYLINDRICAL_SURFACE('',#10369,0.225);
#8524=CYLINDRICAL_SURFACE('',#10376,0.225);
#8525=CYLINDRICAL_SURFACE('',#10380,1.1);
#8526=CYLINDRICAL_SURFACE('',#10386,1.6);
#8527=CYLINDRICAL_SURFACE('',#10390,0.525);
#8528=CYLINDRICAL_SURFACE('',#10394,0.4);
#8529=CYLINDRICAL_SURFACE('',#10399,0.4);
#8530=CYLINDRICAL_SURFACE('',#10404,0.4);
#8531=CYLINDRICAL_SURFACE('',#10409,0.4);
#8532=CYLINDRICAL_SURFACE('',#10414,0.225);
#8533=CYLINDRICAL_SURFACE('',#10416,0.225);
#8534=CYLINDRICAL_SURFACE('',#10418,0.225);
#8535=CYLINDRICAL_SURFACE('',#10420,0.225);
#8536=CYLINDRICAL_SURFACE('',#10440,1.05);
#8537=CYLINDRICAL_SURFACE('',#10444,1.);
#8538=CYLINDRICAL_SURFACE('',#10448,1.05);
#8539=CYLINDRICAL_SURFACE('',#10452,1.);
#8540=CYLINDRICAL_SURFACE('',#10456,1.05);
#8541=CYLINDRICAL_SURFACE('',#10460,0.9);
#8542=CYLINDRICAL_SURFACE('',#10473,0.895);
#8543=CYLINDRICAL_SURFACE('',#10477,0.605);
#8544=CYLINDRICAL_SURFACE('',#10495,0.35);
#8545=CYLINDRICAL_SURFACE('',#10503,0.1954);
#8546=CYLINDRICAL_SURFACE('',#10506,0.165);
#8547=CYLINDRICAL_SURFACE('',#10510,0.165);
#8548=CYLINDRICAL_SURFACE('',#10520,0.8);
#8549=CYLINDRICAL_SURFACE('',#10521,0.6);
#8550=CYLINDRICAL_SURFACE('',#10528,0.8);
#8551=CYLINDRICAL_SURFACE('',#10529,0.6);
#8552=CYLINDRICAL_SURFACE('',#10531,0.6);
#8553=CYLINDRICAL_SURFACE('',#10536,0.605);
#8554=CYLINDRICAL_SURFACE('',#10539,0.8);
#8555=CYLINDRICAL_SURFACE('',#10545,0.605);
#8556=CYLINDRICAL_SURFACE('',#10548,0.8);
#8557=CYLINDRICAL_SURFACE('',#10554,2.3);
#8558=CYLINDRICAL_SURFACE('',#10559,0.164999999999999);
#8559=CYLINDRICAL_SURFACE('',#10564,0.6);
#8560=CYLINDRICAL_SURFACE('',#10567,1.2);
#8561=CYLINDRICAL_SURFACE('',#10572,0.225);
#8562=CYLINDRICAL_SURFACE('',#10575,1.);
#8563=CYLINDRICAL_SURFACE('',#10581,0.225);
#8564=CYLINDRICAL_SURFACE('',#10584,1.);
#8565=CYLINDRICAL_SURFACE('',#10592,0.164999999999999);
#8566=CYLINDRICAL_SURFACE('',#10595,0.605);
#8567=CYLINDRICAL_SURFACE('',#10598,1.);
#8568=CYLINDRICAL_SURFACE('',#10608,0.35);
#8569=CYLINDRICAL_SURFACE('',#10616,0.1954);
#8570=CYLINDRICAL_SURFACE('',#10683,0.1954);
#8571=ADVANCED_FACE('',(#1273),#8357,.F.);
#8572=ADVANCED_FACE('',(#1274),#8358,.F.);
#8573=ADVANCED_FACE('',(#1275),#8359,.F.);
#8574=ADVANCED_FACE('',(#1276),#8360,.F.);
#8575=ADVANCED_FACE('',(#1277),#8361,.F.);
#8576=ADVANCED_FACE('',(#1278),#8362,.F.);
#8577=ADVANCED_FACE('',(#1279),#8363,.F.);
#8578=ADVANCED_FACE('',(#1280),#8364,.F.);
#8579=ADVANCED_FACE('',(#1281),#8365,.F.);
#8580=ADVANCED_FACE('',(#1282),#8366,.F.);
#8581=ADVANCED_FACE('',(#1283),#8367,.F.);
#8582=ADVANCED_FACE('',(#1284),#8368,.F.);
#8583=ADVANCED_FACE('',(#1285),#1014,.T.);
#8584=ADVANCED_FACE('',(#1286),#1015,.T.);
#8585=ADVANCED_FACE('',(#1287),#1016,.T.);
#8586=ADVANCED_FACE('',(#1288),#1017,.T.);
#8587=ADVANCED_FACE('',(#1289,#718,#719,#720,#721,#722,#723,#724,#725,#726,
#727,#728,#729),#1018,.T.);
#8588=ADVANCED_FACE('',(#1290,#730,#731,#732,#733,#734,#735,#736,#737,#738,
#739,#740,#741),#1019,.F.);
#8589=ADVANCED_FACE('',(#1291),#1020,.T.);
#8590=ADVANCED_FACE('',(#1292),#1021,.T.);
#8591=ADVANCED_FACE('',(#1293),#1022,.T.);
#8592=ADVANCED_FACE('',(#1294),#1023,.T.);
#8593=ADVANCED_FACE('',(#1295),#1024,.T.);
#8594=ADVANCED_FACE('',(#1296),#1025,.F.);
#8595=ADVANCED_FACE('',(#1297),#1026,.T.);
#8596=ADVANCED_FACE('',(#1298),#1027,.T.);
#8597=ADVANCED_FACE('',(#1299),#1028,.T.);
#8598=ADVANCED_FACE('',(#1300),#1029,.T.);
#8599=ADVANCED_FACE('',(#1301),#1030,.T.);
#8600=ADVANCED_FACE('',(#1302),#1031,.F.);
#8601=ADVANCED_FACE('',(#1303),#8369,.F.);
#8602=ADVANCED_FACE('',(#1304),#8370,.F.);
#8603=ADVANCED_FACE('',(#1305),#1032,.T.);
#8604=ADVANCED_FACE('',(#1306),#8371,.F.);
#8605=ADVANCED_FACE('',(#1307),#1033,.T.);
#8606=ADVANCED_FACE('',(#1308),#8372,.F.);
#8607=ADVANCED_FACE('',(#1309,#742),#1034,.T.);
#8608=ADVANCED_FACE('',(#1310),#8373,.F.);
#8609=ADVANCED_FACE('',(#1311,#743),#1035,.T.);
#8610=ADVANCED_FACE('',(#1312,#744),#1036,.T.);
#8611=ADVANCED_FACE('',(#1313),#8374,.F.);
#8612=ADVANCED_FACE('',(#1314),#8375,.F.);
#8613=ADVANCED_FACE('',(#1315),#8376,.F.);
#8614=ADVANCED_FACE('',(#1316),#1037,.T.);
#8615=ADVANCED_FACE('',(#1317,#745),#1038,.T.);
#8616=ADVANCED_FACE('',(#1318),#1039,.T.);
#8617=ADVANCED_FACE('',(#1319,#746),#1040,.T.);
#8618=ADVANCED_FACE('',(#1320,#747,#748),#1041,.F.);
#8619=ADVANCED_FACE('',(#1321),#8377,.F.);
#8620=ADVANCED_FACE('',(#1322),#8378,.F.);
#8621=ADVANCED_FACE('',(#1323),#1042,.T.);
#8622=ADVANCED_FACE('',(#1324),#8379,.F.);
#8623=ADVANCED_FACE('',(#1325),#1043,.T.);
#8624=ADVANCED_FACE('',(#1326),#8380,.F.);
#8625=ADVANCED_FACE('',(#1327,#749),#1044,.T.);
#8626=ADVANCED_FACE('',(#1328),#8381,.F.);
#8627=ADVANCED_FACE('',(#1329,#750),#1045,.T.);
#8628=ADVANCED_FACE('',(#1330,#751),#1046,.T.);
#8629=ADVANCED_FACE('',(#1331),#8382,.F.);
#8630=ADVANCED_FACE('',(#1332),#8383,.F.);
#8631=ADVANCED_FACE('',(#1333),#8384,.F.);
#8632=ADVANCED_FACE('',(#1334),#1047,.T.);
#8633=ADVANCED_FACE('',(#1335,#752),#1048,.T.);
#8634=ADVANCED_FACE('',(#1336),#1049,.T.);
#8635=ADVANCED_FACE('',(#1337,#753),#1050,.T.);
#8636=ADVANCED_FACE('',(#1338,#754,#755),#1051,.F.);
#8637=ADVANCED_FACE('',(#1339),#8385,.F.);
#8638=ADVANCED_FACE('',(#1340),#8386,.F.);
#8639=ADVANCED_FACE('',(#1341),#1052,.T.);
#8640=ADVANCED_FACE('',(#1342),#8387,.F.);
#8641=ADVANCED_FACE('',(#1343),#1053,.T.);
#8642=ADVANCED_FACE('',(#1344),#8388,.F.);
#8643=ADVANCED_FACE('',(#1345,#756),#1054,.T.);
#8644=ADVANCED_FACE('',(#1346),#8389,.F.);
#8645=ADVANCED_FACE('',(#1347,#757),#1055,.T.);
#8646=ADVANCED_FACE('',(#1348,#758),#1056,.T.);
#8647=ADVANCED_FACE('',(#1349),#8390,.F.);
#8648=ADVANCED_FACE('',(#1350),#8391,.F.);
#8649=ADVANCED_FACE('',(#1351),#8392,.F.);
#8650=ADVANCED_FACE('',(#1352),#1057,.T.);
#8651=ADVANCED_FACE('',(#1353,#759),#1058,.T.);
#8652=ADVANCED_FACE('',(#1354),#1059,.T.);
#8653=ADVANCED_FACE('',(#1355,#760),#1060,.T.);
#8654=ADVANCED_FACE('',(#1356,#761,#762),#1061,.F.);
#8655=ADVANCED_FACE('',(#1357),#8393,.F.);
#8656=ADVANCED_FACE('',(#1358),#8394,.F.);
#8657=ADVANCED_FACE('',(#1359),#1062,.T.);
#8658=ADVANCED_FACE('',(#1360),#8395,.F.);
#8659=ADVANCED_FACE('',(#1361),#1063,.T.);
#8660=ADVANCED_FACE('',(#1362),#8396,.F.);
#8661=ADVANCED_FACE('',(#1363,#763),#1064,.T.);
#8662=ADVANCED_FACE('',(#1364),#8397,.F.);
#8663=ADVANCED_FACE('',(#1365,#764),#1065,.T.);
#8664=ADVANCED_FACE('',(#1366,#765),#1066,.T.);
#8665=ADVANCED_FACE('',(#1367),#8398,.F.);
#8666=ADVANCED_FACE('',(#1368),#8399,.F.);
#8667=ADVANCED_FACE('',(#1369),#8400,.F.);
#8668=ADVANCED_FACE('',(#1370),#1067,.T.);
#8669=ADVANCED_FACE('',(#1371,#766),#1068,.T.);
#8670=ADVANCED_FACE('',(#1372),#1069,.T.);
#8671=ADVANCED_FACE('',(#1373,#767),#1070,.T.);
#8672=ADVANCED_FACE('',(#1374,#768,#769),#1071,.F.);
#8673=ADVANCED_FACE('',(#1375),#8401,.F.);
#8674=ADVANCED_FACE('',(#1376),#8402,.F.);
#8675=ADVANCED_FACE('',(#1377),#8403,.F.);
#8676=ADVANCED_FACE('',(#1378),#8404,.F.);
#8677=ADVANCED_FACE('',(#1379),#8405,.F.);
#8678=ADVANCED_FACE('',(#1380),#8406,.F.);
#8679=ADVANCED_FACE('',(#1381),#8407,.F.);
#8680=ADVANCED_FACE('',(#1382,#770),#1072,.T.);
#8681=ADVANCED_FACE('',(#1383,#771),#1073,.T.);
#8682=ADVANCED_FACE('',(#1384),#1074,.T.);
#8683=ADVANCED_FACE('',(#1385),#1075,.T.);
#8684=ADVANCED_FACE('',(#1386),#1076,.T.);
#8685=ADVANCED_FACE('',(#1387,#772,#773,#774,#775,#776),#1077,.T.);
#8686=ADVANCED_FACE('',(#1388),#1078,.T.);
#8687=ADVANCED_FACE('',(#1389,#777,#778,#779,#780,#781),#1079,.T.);
#8688=ADVANCED_FACE('',(#1390),#1080,.T.);
#8689=ADVANCED_FACE('',(#1391,#782,#783),#1081,.F.);
#8690=ADVANCED_FACE('',(#1392),#8408,.F.);
#8691=ADVANCED_FACE('',(#1393),#8409,.F.);
#8692=ADVANCED_FACE('',(#1394),#8410,.F.);
#8693=ADVANCED_FACE('',(#1395),#8411,.F.);
#8694=ADVANCED_FACE('',(#1396),#8412,.T.);
#8695=ADVANCED_FACE('',(#1397,#784),#1082,.T.);
#8696=ADVANCED_FACE('',(#1398),#8413,.F.);
#8697=ADVANCED_FACE('',(#1399),#8414,.T.);
#8698=ADVANCED_FACE('',(#1400,#785,#786,#787,#788,#789),#1083,.T.);
#8699=ADVANCED_FACE('',(#1401,#790,#791,#792,#793,#794),#1084,.F.);
#8700=ADVANCED_FACE('',(#1402),#8415,.F.);
#8701=ADVANCED_FACE('',(#1403),#8416,.F.);
#8702=ADVANCED_FACE('',(#1404),#8417,.F.);
#8703=ADVANCED_FACE('',(#1405),#8418,.F.);
#8704=ADVANCED_FACE('',(#1406),#8419,.T.);
#8705=ADVANCED_FACE('',(#1407,#795),#1085,.F.);
#8706=ADVANCED_FACE('',(#1408),#8420,.F.);
#8707=ADVANCED_FACE('',(#1409),#8421,.T.);
#8708=ADVANCED_FACE('',(#1410,#796,#797,#798,#799,#800),#1086,.T.);
#8709=ADVANCED_FACE('',(#1411,#801,#802,#803,#804,#805),#1087,.F.);
#8710=ADVANCED_FACE('',(#1412),#8422,.F.);
#8711=ADVANCED_FACE('',(#1413),#8423,.F.);
#8712=ADVANCED_FACE('',(#1414),#8424,.F.);
#8713=ADVANCED_FACE('',(#1415),#8425,.F.);
#8714=ADVANCED_FACE('',(#1416),#8426,.F.);
#8715=ADVANCED_FACE('',(#1417),#8427,.F.);
#8716=ADVANCED_FACE('',(#1418),#8428,.F.);
#8717=ADVANCED_FACE('',(#1419,#806),#1088,.T.);
#8718=ADVANCED_FACE('',(#1420,#807),#1089,.T.);
#8719=ADVANCED_FACE('',(#1421),#1090,.T.);
#8720=ADVANCED_FACE('',(#1422),#1091,.T.);
#8721=ADVANCED_FACE('',(#1423),#1092,.T.);
#8722=ADVANCED_FACE('',(#1424,#808,#809,#810,#811,#812),#1093,.T.);
#8723=ADVANCED_FACE('',(#1425),#1094,.T.);
#8724=ADVANCED_FACE('',(#1426,#813,#814,#815,#816,#817),#1095,.T.);
#8725=ADVANCED_FACE('',(#1427),#1096,.T.);
#8726=ADVANCED_FACE('',(#1428,#818,#819),#1097,.F.);
#8727=ADVANCED_FACE('',(#1429),#8429,.F.);
#8728=ADVANCED_FACE('',(#1430),#8430,.F.);
#8729=ADVANCED_FACE('',(#1431),#8431,.F.);
#8730=ADVANCED_FACE('',(#1432),#8432,.F.);
#8731=ADVANCED_FACE('',(#1433),#8433,.T.);
#8732=ADVANCED_FACE('',(#1434,#820),#1098,.T.);
#8733=ADVANCED_FACE('',(#1435),#8434,.F.);
#8734=ADVANCED_FACE('',(#1436),#8435,.T.);
#8735=ADVANCED_FACE('',(#1437,#821,#822,#823,#824,#825),#1099,.T.);
#8736=ADVANCED_FACE('',(#1438,#826,#827,#828,#829,#830),#1100,.F.);
#8737=ADVANCED_FACE('',(#1439),#8436,.F.);
#8738=ADVANCED_FACE('',(#1440),#8437,.F.);
#8739=ADVANCED_FACE('',(#1441),#8438,.F.);
#8740=ADVANCED_FACE('',(#1442),#8439,.F.);
#8741=ADVANCED_FACE('',(#1443),#8440,.T.);
#8742=ADVANCED_FACE('',(#1444,#831),#1101,.F.);
#8743=ADVANCED_FACE('',(#1445),#8441,.F.);
#8744=ADVANCED_FACE('',(#1446),#8442,.T.);
#8745=ADVANCED_FACE('',(#1447,#832,#833,#834,#835,#836),#1102,.T.);
#8746=ADVANCED_FACE('',(#1448,#837,#838,#839,#840,#841),#1103,.F.);
#8747=ADVANCED_FACE('',(#1449),#483,.T.);
#8748=ADVANCED_FACE('',(#1450),#8443,.T.);
#8749=ADVANCED_FACE('',(#1451),#1104,.F.);
#8750=ADVANCED_FACE('',(#1452),#484,.T.);
#8751=ADVANCED_FACE('',(#1453),#1105,.T.);
#8752=ADVANCED_FACE('',(#1454),#481,.F.);
#8753=ADVANCED_FACE('',(#1455),#8444,.T.);
#8754=ADVANCED_FACE('',(#1456),#8445,.F.);
#8755=ADVANCED_FACE('',(#1457),#485,.F.);
#8756=ADVANCED_FACE('',(#1458,#842),#1106,.T.);
#8757=ADVANCED_FACE('',(#1459),#8446,.T.);
#8758=ADVANCED_FACE('',(#1460,#843),#1107,.T.);
#8759=ADVANCED_FACE('',(#1461),#486,.F.);
#8760=ADVANCED_FACE('',(#1462),#482,.F.);
#8761=ADVANCED_FACE('',(#1463),#8447,.F.);
#8762=ADVANCED_FACE('',(#1464,#844),#1108,.T.);
#8763=ADVANCED_FACE('',(#1465),#487,.T.);
#8764=ADVANCED_FACE('',(#1466),#8448,.T.);
#8765=ADVANCED_FACE('',(#1467),#488,.T.);
#8766=ADVANCED_FACE('',(#1468,#845),#1109,.T.);
#8767=ADVANCED_FACE('',(#1469),#8449,.F.);
#8768=ADVANCED_FACE('',(#1470),#467,.T.);
#8769=ADVANCED_FACE('',(#1471),#468,.T.);
#8770=ADVANCED_FACE('',(#1472),#469,.T.);
#8771=ADVANCED_FACE('',(#1473),#470,.T.);
#8772=ADVANCED_FACE('',(#1474),#471,.T.);
#8773=ADVANCED_FACE('',(#1475),#472,.T.);
#8774=ADVANCED_FACE('',(#1476),#473,.T.);
#8775=ADVANCED_FACE('',(#1477),#474,.F.);
#8776=ADVANCED_FACE('',(#1478),#8450,.T.);
#8777=ADVANCED_FACE('',(#1479),#1110,.T.);
#8778=ADVANCED_FACE('',(#1480),#475,.F.);
#8779=ADVANCED_FACE('',(#1481),#1111,.T.);
#8780=ADVANCED_FACE('',(#1482),#476,.F.);
#8781=ADVANCED_FACE('',(#1483),#1112,.T.);
#8782=ADVANCED_FACE('',(#1484),#477,.F.);
#8783=ADVANCED_FACE('',(#1485),#1113,.T.);
#8784=ADVANCED_FACE('',(#1486),#478,.F.);
#8785=ADVANCED_FACE('',(#1487),#1114,.T.);
#8786=ADVANCED_FACE('',(#1488),#479,.F.);
#8787=ADVANCED_FACE('',(#1489),#8451,.F.);
#8788=ADVANCED_FACE('',(#1490),#1115,.T.);
#8789=ADVANCED_FACE('',(#1491),#480,.F.);
#8790=ADVANCED_FACE('',(#1492,#846),#1116,.T.);
#8791=ADVANCED_FACE('',(#1493),#1117,.T.);
#8792=ADVANCED_FACE('',(#1494,#847),#1118,.T.);
#8793=ADVANCED_FACE('',(#1495),#8452,.T.);
#8794=ADVANCED_FACE('',(#1496,#848),#1119,.T.);
#8795=ADVANCED_FACE('',(#1497),#8453,.F.);
#8796=ADVANCED_FACE('',(#1498,#849),#1120,.T.);
#8797=ADVANCED_FACE('',(#1499),#8454,.T.);
#8798=ADVANCED_FACE('',(#1500,#850),#1121,.T.);
#8799=ADVANCED_FACE('',(#1501),#8455,.F.);
#8800=ADVANCED_FACE('',(#1502),#8456,.F.);
#8801=ADVANCED_FACE('',(#1503),#1122,.T.);
#8802=ADVANCED_FACE('',(#1504),#8457,.F.);
#8803=ADVANCED_FACE('',(#1505),#1123,.T.);
#8804=ADVANCED_FACE('',(#1506),#8458,.F.);
#8805=ADVANCED_FACE('',(#1507),#1124,.T.);
#8806=ADVANCED_FACE('',(#1508),#8459,.F.);
#8807=ADVANCED_FACE('',(#1509),#1125,.T.);
#8808=ADVANCED_FACE('',(#1510),#8460,.F.);
#8809=ADVANCED_FACE('',(#1511),#1126,.T.);
#8810=ADVANCED_FACE('',(#1512),#8461,.F.);
#8811=ADVANCED_FACE('',(#1513),#1127,.T.);
#8812=ADVANCED_FACE('',(#1514),#8462,.F.);
#8813=ADVANCED_FACE('',(#1515),#8463,.F.);
#8814=ADVANCED_FACE('',(#1516),#8464,.F.);
#8815=ADVANCED_FACE('',(#1517),#8465,.F.);
#8816=ADVANCED_FACE('',(#1518),#8466,.F.);
#8817=ADVANCED_FACE('',(#1519),#8467,.F.);
#8818=ADVANCED_FACE('',(#1520),#8468,.F.);
#8819=ADVANCED_FACE('',(#1521),#1128,.T.);
#8820=ADVANCED_FACE('',(#1522,#851,#852,#853,#854,#855,#856,#857,#858,#859,
#860,#861,#862,#863),#1129,.T.);
#8821=ADVANCED_FACE('',(#1523),#1130,.T.);
#8822=ADVANCED_FACE('',(#1524,#864,#865,#866,#867,#868,#869,#870),#1131,
 .T.);
#8823=ADVANCED_FACE('',(#1525),#1132,.T.);
#8824=ADVANCED_FACE('',(#1526),#1133,.F.);
#8825=ADVANCED_FACE('',(#1527),#8469,.F.);
#8826=ADVANCED_FACE('',(#1528),#8470,.F.);
#8827=ADVANCED_FACE('',(#1529),#8471,.F.);
#8828=ADVANCED_FACE('',(#1530),#8472,.F.);
#8829=ADVANCED_FACE('',(#1531),#8473,.F.);
#8830=ADVANCED_FACE('',(#1532),#8474,.F.);
#8831=ADVANCED_FACE('',(#1533),#8475,.F.);
#8832=ADVANCED_FACE('',(#1534),#1134,.T.);
#8833=ADVANCED_FACE('',(#1535,#871,#872,#873,#874,#875,#876,#877),#1135,
 .T.);
#8834=ADVANCED_FACE('',(#1536),#1136,.T.);
#8835=ADVANCED_FACE('',(#1537,#878,#879,#880,#881,#882,#883,#884),#1137,
 .T.);
#8836=ADVANCED_FACE('',(#1538),#1138,.T.);
#8837=ADVANCED_FACE('',(#1539),#1139,.F.);
#8838=ADVANCED_FACE('',(#1540),#8476,.F.);
#8839=ADVANCED_FACE('',(#1541),#8477,.F.);
#8840=ADVANCED_FACE('',(#1542),#8478,.F.);
#8841=ADVANCED_FACE('',(#1543),#8479,.F.);
#8842=ADVANCED_FACE('',(#1544),#8480,.F.);
#8843=ADVANCED_FACE('',(#1545),#8481,.F.);
#8844=ADVANCED_FACE('',(#1546),#8482,.F.);
#8845=ADVANCED_FACE('',(#1547),#1140,.T.);
#8846=ADVANCED_FACE('',(#1548,#885,#886,#887,#888,#889,#890,#891),#1141,
 .T.);
#8847=ADVANCED_FACE('',(#1549),#1142,.T.);
#8848=ADVANCED_FACE('',(#1550,#892,#893,#894,#895,#896,#897,#898),#1143,
 .T.);
#8849=ADVANCED_FACE('',(#1551),#1144,.T.);
#8850=ADVANCED_FACE('',(#1552),#1145,.F.);
#8851=ADVANCED_FACE('',(#1553),#1146,.T.);
#8852=ADVANCED_FACE('',(#1554),#8483,.F.);
#8853=ADVANCED_FACE('',(#1555),#1147,.T.);
#8854=ADVANCED_FACE('',(#1556),#8484,.F.);
#8855=ADVANCED_FACE('',(#1557),#8485,.T.);
#8856=ADVANCED_FACE('',(#1558,#899),#1148,.F.);
#8857=ADVANCED_FACE('',(#1559),#8486,.T.);
#8858=ADVANCED_FACE('',(#1560,#900,#901,#902),#1149,.T.);
#8859=ADVANCED_FACE('',(#1561),#8487,.F.);
#8860=ADVANCED_FACE('',(#1562,#903),#1150,.F.);
#8861=ADVANCED_FACE('',(#1563),#8488,.F.);
#8862=ADVANCED_FACE('',(#1564,#904),#1151,.T.);
#8863=ADVANCED_FACE('',(#1565),#8489,.F.);
#8864=ADVANCED_FACE('',(#1566,#905),#1152,.T.);
#8865=ADVANCED_FACE('',(#1567),#8490,.F.);
#8866=ADVANCED_FACE('',(#1568,#906),#1153,.T.);
#8867=ADVANCED_FACE('',(#1569),#8491,.F.);
#8868=ADVANCED_FACE('',(#1570,#907),#1154,.T.);
#8869=ADVANCED_FACE('',(#1571),#8492,.F.);
#8870=ADVANCED_FACE('',(#1572),#8493,.F.);
#8871=ADVANCED_FACE('',(#1573),#8494,.F.);
#8872=ADVANCED_FACE('',(#1574),#8495,.F.);
#8873=ADVANCED_FACE('',(#1575),#1155,.T.);
#8874=ADVANCED_FACE('',(#1576,#908,#909,#910,#911),#1156,.T.);
#8875=ADVANCED_FACE('',(#1577),#1157,.T.);
#8876=ADVANCED_FACE('',(#1578,#912,#913,#914,#915),#1158,.T.);
#8877=ADVANCED_FACE('',(#1579),#1159,.T.);
#8878=ADVANCED_FACE('',(#1580),#1160,.F.);
#8879=ADVANCED_FACE('',(#1581),#8496,.F.);
#8880=ADVANCED_FACE('',(#1582),#1161,.F.);
#8881=ADVANCED_FACE('',(#1583),#8497,.F.);
#8882=ADVANCED_FACE('',(#1584),#1162,.F.);
#8883=ADVANCED_FACE('',(#1585),#8498,.F.);
#8884=ADVANCED_FACE('',(#1586),#1163,.F.);
#8885=ADVANCED_FACE('',(#1587),#8499,.F.);
#8886=ADVANCED_FACE('',(#1588),#1164,.F.);
#8887=ADVANCED_FACE('',(#1589),#8500,.F.);
#8888=ADVANCED_FACE('',(#1590),#1165,.F.);
#8889=ADVANCED_FACE('',(#1591),#8501,.F.);
#8890=ADVANCED_FACE('',(#1592),#1166,.F.);
#8891=ADVANCED_FACE('',(#1593),#8502,.F.);
#8892=ADVANCED_FACE('',(#1594),#8503,.F.);
#8893=ADVANCED_FACE('',(#1595),#8504,.F.);
#8894=ADVANCED_FACE('',(#1596),#8505,.F.);
#8895=ADVANCED_FACE('',(#1597),#8506,.F.);
#8896=ADVANCED_FACE('',(#1598),#8507,.F.);
#8897=ADVANCED_FACE('',(#1599),#8508,.F.);
#8898=ADVANCED_FACE('',(#1600),#1167,.T.);
#8899=ADVANCED_FACE('',(#1601,#916,#917,#918,#919,#920,#921,#922),#1168,
 .T.);
#8900=ADVANCED_FACE('',(#1602),#1169,.T.);
#8901=ADVANCED_FACE('',(#1603,#923,#924,#925,#926,#927,#928,#929,#930,#931,
#932,#933,#934,#935),#1170,.T.);
#8902=ADVANCED_FACE('',(#1604),#1171,.T.);
#8903=ADVANCED_FACE('',(#1605),#1172,.F.);
#8904=ADVANCED_FACE('',(#1606),#8509,.F.);
#8905=ADVANCED_FACE('',(#1607),#8510,.F.);
#8906=ADVANCED_FACE('',(#1608),#8511,.F.);
#8907=ADVANCED_FACE('',(#1609),#8512,.F.);
#8908=ADVANCED_FACE('',(#1610),#8513,.F.);
#8909=ADVANCED_FACE('',(#1611),#8514,.F.);
#8910=ADVANCED_FACE('',(#1612),#8515,.F.);
#8911=ADVANCED_FACE('',(#1613),#1173,.T.);
#8912=ADVANCED_FACE('',(#1614,#936,#937,#938,#939,#940,#941,#942),#1174,
 .T.);
#8913=ADVANCED_FACE('',(#1615),#1175,.T.);
#8914=ADVANCED_FACE('',(#1616,#943,#944,#945,#946,#947,#948,#949),#1176,
 .T.);
#8915=ADVANCED_FACE('',(#1617),#1177,.T.);
#8916=ADVANCED_FACE('',(#1618),#1178,.F.);
#8917=ADVANCED_FACE('',(#1619),#8516,.F.);
#8918=ADVANCED_FACE('',(#1620),#8517,.F.);
#8919=ADVANCED_FACE('',(#1621),#8518,.F.);
#8920=ADVANCED_FACE('',(#1622),#8519,.F.);
#8921=ADVANCED_FACE('',(#1623),#8520,.F.);
#8922=ADVANCED_FACE('',(#1624),#8521,.F.);
#8923=ADVANCED_FACE('',(#1625),#8522,.F.);
#8924=ADVANCED_FACE('',(#1626),#1179,.T.);
#8925=ADVANCED_FACE('',(#1627,#950,#951,#952,#953,#954,#955,#956),#1180,
 .T.);
#8926=ADVANCED_FACE('',(#1628),#1181,.T.);
#8927=ADVANCED_FACE('',(#1629,#957,#958,#959,#960,#961,#962,#963),#1182,
 .T.);
#8928=ADVANCED_FACE('',(#1630),#1183,.T.);
#8929=ADVANCED_FACE('',(#1631),#1184,.F.);
#8930=ADVANCED_FACE('',(#1632),#1185,.F.);
#8931=ADVANCED_FACE('',(#1633),#8523,.F.);
#8932=ADVANCED_FACE('',(#1634),#1186,.F.);
#8933=ADVANCED_FACE('',(#1635),#8524,.F.);
#8934=ADVANCED_FACE('',(#1636),#8525,.T.);
#8935=ADVANCED_FACE('',(#1637,#964),#1187,.T.);
#8936=ADVANCED_FACE('',(#1638),#8526,.T.);
#8937=ADVANCED_FACE('',(#1639,#965,#966,#967),#1188,.F.);
#8938=ADVANCED_FACE('',(#1640),#8527,.F.);
#8939=ADVANCED_FACE('',(#1641,#968),#1189,.T.);
#8940=ADVANCED_FACE('',(#1642),#8528,.F.);
#8941=ADVANCED_FACE('',(#1643,#969),#1190,.F.);
#8942=ADVANCED_FACE('',(#1644),#8529,.F.);
#8943=ADVANCED_FACE('',(#1645,#970),#1191,.F.);
#8944=ADVANCED_FACE('',(#1646),#8530,.F.);
#8945=ADVANCED_FACE('',(#1647,#971),#1192,.F.);
#8946=ADVANCED_FACE('',(#1648),#8531,.F.);
#8947=ADVANCED_FACE('',(#1649,#972),#1193,.F.);
#8948=ADVANCED_FACE('',(#1650),#8532,.F.);
#8949=ADVANCED_FACE('',(#1651),#8533,.F.);
#8950=ADVANCED_FACE('',(#1652),#8534,.F.);
#8951=ADVANCED_FACE('',(#1653),#8535,.F.);
#8952=ADVANCED_FACE('',(#1654),#1194,.T.);
#8953=ADVANCED_FACE('',(#1655,#973,#974,#975,#976),#1195,.T.);
#8954=ADVANCED_FACE('',(#1656),#1196,.T.);
#8955=ADVANCED_FACE('',(#1657,#977,#978,#979,#980),#1197,.T.);
#8956=ADVANCED_FACE('',(#1658),#1198,.T.);
#8957=ADVANCED_FACE('',(#1659),#1199,.F.);
#8958=ADVANCED_FACE('',(#1660),#1200,.F.);
#8959=ADVANCED_FACE('',(#1661),#1201,.F.);
#8960=ADVANCED_FACE('',(#1662),#1202,.F.);
#8961=ADVANCED_FACE('',(#1663),#1203,.F.);
#8962=ADVANCED_FACE('',(#1664),#1204,.F.);
#8963=ADVANCED_FACE('',(#1665,#981),#1205,.T.);
#8964=ADVANCED_FACE('',(#1666),#8536,.T.);
#8965=ADVANCED_FACE('',(#1667,#982),#1206,.T.);
#8966=ADVANCED_FACE('',(#1668),#8537,.T.);
#8967=ADVANCED_FACE('',(#1669,#983),#1207,.T.);
#8968=ADVANCED_FACE('',(#1670),#8538,.T.);
#8969=ADVANCED_FACE('',(#1671,#984),#1208,.T.);
#8970=ADVANCED_FACE('',(#1672),#8539,.T.);
#8971=ADVANCED_FACE('',(#1673,#985),#1209,.T.);
#8972=ADVANCED_FACE('',(#1674),#8540,.T.);
#8973=ADVANCED_FACE('',(#1675,#986),#1210,.T.);
#8974=ADVANCED_FACE('',(#1676,#987),#8541,.F.);
#8975=ADVANCED_FACE('',(#1677),#1211,.F.);
#8976=ADVANCED_FACE('',(#1678),#1212,.F.);
#8977=ADVANCED_FACE('',(#1679),#1213,.F.);
#8978=ADVANCED_FACE('',(#1680),#1214,.F.);
#8979=ADVANCED_FACE('',(#1681,#988),#1215,.T.);
#8980=ADVANCED_FACE('',(#1682,#989),#8542,.T.);
#8981=ADVANCED_FACE('',(#1683,#990),#1216,.T.);
#8982=ADVANCED_FACE('',(#1684,#991),#8543,.F.);
#8983=ADVANCED_FACE('',(#1685),#1217,.F.);
#8984=ADVANCED_FACE('',(#1686),#1218,.F.);
#8985=ADVANCED_FACE('',(#1687),#1219,.F.);
#8986=ADVANCED_FACE('',(#1688),#1220,.F.);
#8987=ADVANCED_FACE('',(#1689),#1221,.F.);
#8988=ADVANCED_FACE('',(#1690),#1222,.F.);
#8989=ADVANCED_FACE('',(#1691),#1223,.F.);
#8990=ADVANCED_FACE('',(#1692),#1224,.F.);
#8991=ADVANCED_FACE('',(#1693),#1225,.F.);
#8992=ADVANCED_FACE('',(#1694),#1226,.T.);
#8993=ADVANCED_FACE('',(#1695),#489,.T.);
#8994=ADVANCED_FACE('',(#1696),#8544,.T.);
#8995=ADVANCED_FACE('',(#1697),#490,.T.);
#8996=ADVANCED_FACE('',(#1698,#992),#1227,.T.);
#8997=ADVANCED_FACE('',(#1699),#491,.T.);
#8998=ADVANCED_FACE('',(#1700),#8545,.T.);
#8999=ADVANCED_FACE('',(#1701),#8546,.F.);
#9000=ADVANCED_FACE('',(#1702),#1228,.T.);
#9001=ADVANCED_FACE('',(#1703),#8547,.F.);
#9002=ADVANCED_FACE('',(#1704),#1229,.F.);
#9003=ADVANCED_FACE('',(#1705,#993),#1230,.T.);
#9004=ADVANCED_FACE('',(#1706,#994),#1231,.F.);
#9005=ADVANCED_FACE('',(#1707),#8548,.T.);
#9006=ADVANCED_FACE('',(#1708),#8549,.T.);
#9007=ADVANCED_FACE('',(#1709,#995),#1232,.T.);
#9008=ADVANCED_FACE('',(#1710,#996),#1233,.F.);
#9009=ADVANCED_FACE('',(#1711),#8550,.T.);
#9010=ADVANCED_FACE('',(#1712),#8551,.T.);
#9011=ADVANCED_FACE('',(#1713),#8552,.T.);
#9012=ADVANCED_FACE('',(#1714,#997),#1234,.T.);
#9013=ADVANCED_FACE('',(#1715,#998),#1235,.F.);
#9014=ADVANCED_FACE('',(#1716),#8553,.F.);
#9015=ADVANCED_FACE('',(#1717),#8554,.T.);
#9016=ADVANCED_FACE('',(#1718,#999),#1236,.T.);
#9017=ADVANCED_FACE('',(#1719,#1000),#1237,.F.);
#9018=ADVANCED_FACE('',(#1720),#8555,.F.);
#9019=ADVANCED_FACE('',(#1721),#8556,.T.);
#9020=ADVANCED_FACE('',(#1722,#1001),#1238,.T.);
#9021=ADVANCED_FACE('',(#1723,#1002),#1239,.F.);
#9022=ADVANCED_FACE('',(#1724),#8557,.T.);
#9023=ADVANCED_FACE('',(#1725),#1240,.T.);
#9024=ADVANCED_FACE('',(#1726),#8558,.F.);
#9025=ADVANCED_FACE('',(#1727),#1241,.T.);
#9026=ADVANCED_FACE('',(#1728,#1003),#1242,.T.);
#9027=ADVANCED_FACE('',(#1729),#8559,.F.);
#9028=ADVANCED_FACE('',(#1730),#8560,.T.);
#9029=ADVANCED_FACE('',(#1731,#1004),#1243,.T.);
#9030=ADVANCED_FACE('',(#1732,#1005),#1244,.F.);
#9031=ADVANCED_FACE('',(#1733),#8561,.F.);
#9032=ADVANCED_FACE('',(#1734),#8562,.T.);
#9033=ADVANCED_FACE('',(#1735,#1006),#1245,.T.);
#9034=ADVANCED_FACE('',(#1736,#1007),#1246,.F.);
#9035=ADVANCED_FACE('',(#1737),#8563,.F.);
#9036=ADVANCED_FACE('',(#1738),#8564,.T.);
#9037=ADVANCED_FACE('',(#1739,#1008),#1247,.T.);
#9038=ADVANCED_FACE('',(#1740,#1009),#1248,.F.);
#9039=ADVANCED_FACE('',(#1741),#1249,.T.);
#9040=ADVANCED_FACE('',(#1742),#8565,.F.);
#9041=ADVANCED_FACE('',(#1743),#1250,.T.);
#9042=ADVANCED_FACE('',(#1744),#8566,.F.);
#9043=ADVANCED_FACE('',(#1745),#8567,.T.);
#9044=ADVANCED_FACE('',(#1746,#1010),#1251,.T.);
#9045=ADVANCED_FACE('',(#1747,#1011),#1252,.F.);
#9046=ADVANCED_FACE('',(#1748),#1253,.T.);
#9047=ADVANCED_FACE('',(#1749),#492,.T.);
#9048=ADVANCED_FACE('',(#1750),#8568,.T.);
#9049=ADVANCED_FACE('',(#1751),#493,.T.);
#9050=ADVANCED_FACE('',(#1752,#1012),#1254,.T.);
#9051=ADVANCED_FACE('',(#1753),#494,.T.);
#9052=ADVANCED_FACE('',(#1754),#8569,.T.);
#9053=ADVANCED_FACE('',(#1755),#495,.T.);
#9054=ADVANCED_FACE('',(#1756),#1255,.T.);
#9055=ADVANCED_FACE('',(#1757),#1256,.F.);
#9056=ADVANCED_FACE('',(#1758),#1257,.F.);
#9057=ADVANCED_FACE('',(#1759),#1258,.F.);
#9058=ADVANCED_FACE('',(#1760),#1259,.F.);
#9059=ADVANCED_FACE('',(#1761),#1260,.F.);
#9060=ADVANCED_FACE('',(#1762),#1261,.F.);
#9061=ADVANCED_FACE('',(#1763),#1262,.F.);
#9062=ADVANCED_FACE('',(#1764),#1263,.F.);
#9063=ADVANCED_FACE('',(#1765),#1264,.F.);
#9064=ADVANCED_FACE('',(#1766),#1265,.F.);
#9065=ADVANCED_FACE('',(#1767),#1266,.F.);
#9066=ADVANCED_FACE('',(#1768),#1267,.F.);
#9067=ADVANCED_FACE('',(#1769),#1268,.F.);
#9068=ADVANCED_FACE('',(#1770),#1269,.F.);
#9069=ADVANCED_FACE('',(#1771),#1270,.F.);
#9070=ADVANCED_FACE('',(#1772,#1013),#1271,.T.);
#9071=ADVANCED_FACE('',(#1773),#496,.T.);
#9072=ADVANCED_FACE('',(#1774),#8570,.T.);
#9073=ADVANCED_FACE('',(#1775),#497,.T.);
#9074=ADVANCED_FACE('',(#1776),#1272,.T.);
#9075=CLOSED_SHELL('',(#8571,#8572,#8573,#8574,#8575,#8576,#8577,#8578,
#8579,#8580,#8581,#8582,#8583,#8584,#8585,#8586,#8587,#8588));
#9076=CLOSED_SHELL('',(#8589,#8590,#8591,#8592,#8593,#8594));
#9077=CLOSED_SHELL('',(#8595,#8596,#8597,#8598,#8599,#8600));
#9078=CLOSED_SHELL('',(#8601,#8602,#8603,#8604,#8605,#8606,#8607,#8608,
#8609,#8610,#8611,#8612,#8613,#8614,#8615,#8616,#8617,#8618));
#9079=CLOSED_SHELL('',(#8619,#8620,#8621,#8622,#8623,#8624,#8625,#8626,
#8627,#8628,#8629,#8630,#8631,#8632,#8633,#8634,#8635,#8636));
#9080=CLOSED_SHELL('',(#8637,#8638,#8639,#8640,#8641,#8642,#8643,#8644,
#8645,#8646,#8647,#8648,#8649,#8650,#8651,#8652,#8653,#8654));
#9081=CLOSED_SHELL('',(#8655,#8656,#8657,#8658,#8659,#8660,#8661,#8662,
#8663,#8664,#8665,#8666,#8667,#8668,#8669,#8670,#8671,#8672));
#9082=CLOSED_SHELL('',(#8673,#8674,#8675,#8676,#8677,#8678,#8679,#8680,
#8681,#8682,#8683,#8684,#8685,#8686,#8687,#8688,#8689));
#9083=CLOSED_SHELL('',(#8690,#8691,#8692,#8693,#8694,#8695,#8696,#8697,
#8698,#8699));
#9084=CLOSED_SHELL('',(#8700,#8701,#8702,#8703,#8704,#8705,#8706,#8707,
#8708,#8709));
#9085=CLOSED_SHELL('',(#8710,#8711,#8712,#8713,#8714,#8715,#8716,#8717,
#8718,#8719,#8720,#8721,#8722,#8723,#8724,#8725,#8726));
#9086=CLOSED_SHELL('',(#8727,#8728,#8729,#8730,#8731,#8732,#8733,#8734,
#8735,#8736));
#9087=CLOSED_SHELL('',(#8737,#8738,#8739,#8740,#8741,#8742,#8743,#8744,
#8745,#8746));
#9088=CLOSED_SHELL('',(#8747,#8748,#8749,#8750,#8751));
#9089=CLOSED_SHELL('',(#8752,#8753,#8754,#8755,#8756,#8757,#8758,#8759));
#9090=CLOSED_SHELL('',(#8760,#8761,#8762,#8763,#8764,#8765,#8766,#8767));
#9091=CLOSED_SHELL('',(#8768));
#9092=CLOSED_SHELL('',(#8769));
#9093=CLOSED_SHELL('',(#8770));
#9094=CLOSED_SHELL('',(#8771));
#9095=CLOSED_SHELL('',(#8772));
#9096=CLOSED_SHELL('',(#8773));
#9097=CLOSED_SHELL('',(#8774));
#9098=CLOSED_SHELL('',(#8775,#8776,#8777,#8778,#8779,#8780,#8781,#8782,
#8783,#8784,#8785,#8786,#8787,#8788,#8789,#8790,#8791));
#9099=CLOSED_SHELL('',(#8792,#8793,#8794,#8795));
#9100=CLOSED_SHELL('',(#8796,#8797,#8798,#8799));
#9101=CLOSED_SHELL('',(#8800,#8801,#8802,#8803,#8804,#8805,#8806,#8807,
#8808,#8809,#8810,#8811,#8812,#8813,#8814,#8815,#8816,#8817,#8818,#8819,
#8820,#8821,#8822,#8823,#8824));
#9102=CLOSED_SHELL('',(#8825,#8826,#8827,#8828,#8829,#8830,#8831,#8832,
#8833,#8834,#8835,#8836,#8837));
#9103=CLOSED_SHELL('',(#8838,#8839,#8840,#8841,#8842,#8843,#8844,#8845,
#8846,#8847,#8848,#8849,#8850));
#9104=CLOSED_SHELL('',(#8851,#8852,#8853,#8854,#8855,#8856,#8857,#8858,
#8859,#8860));
#9105=CLOSED_SHELL('',(#8861,#8862,#8863,#8864,#8865,#8866,#8867,#8868,
#8869,#8870,#8871,#8872,#8873,#8874,#8875,#8876,#8877,#8878));
#9106=CLOSED_SHELL('',(#8879,#8880,#8881,#8882,#8883,#8884,#8885,#8886,
#8887,#8888,#8889,#8890,#8891,#8892,#8893,#8894,#8895,#8896,#8897,#8898,
#8899,#8900,#8901,#8902,#8903));
#9107=CLOSED_SHELL('',(#8904,#8905,#8906,#8907,#8908,#8909,#8910,#8911,
#8912,#8913,#8914,#8915,#8916));
#9108=CLOSED_SHELL('',(#8917,#8918,#8919,#8920,#8921,#8922,#8923,#8924,
#8925,#8926,#8927,#8928,#8929));
#9109=CLOSED_SHELL('',(#8930,#8931,#8932,#8933,#8934,#8935,#8936,#8937,
#8938,#8939));
#9110=CLOSED_SHELL('',(#8940,#8941,#8942,#8943,#8944,#8945,#8946,#8947,
#8948,#8949,#8950,#8951,#8952,#8953,#8954,#8955,#8956,#8957));
#9111=CLOSED_SHELL('',(#8958,#8959,#8960,#8961,#8962,#8963,#8964,#8965,
#8966,#8967,#8968,#8969,#8970,#8971,#8972,#8973,#8974));
#9112=CLOSED_SHELL('',(#8975,#8976,#8977,#8978,#8979,#8980,#8981,#8982));
#9113=CLOSED_SHELL('',(#8983,#8984,#8985,#8986,#8987,#8988,#8989,#8990));
#9114=CLOSED_SHELL('',(#8991,#8992,#8993,#8994,#8995,#8996,#8997,#8998));
#9115=CLOSED_SHELL('',(#8999,#9000,#9001,#9002,#9003,#9004,#9005,#9006,
#9007,#9008,#9009,#9010,#9011,#9012,#9013));
#9116=CLOSED_SHELL('',(#9014,#9015,#9016,#9017));
#9117=CLOSED_SHELL('',(#9018,#9019,#9020,#9021));
#9118=CLOSED_SHELL('',(#9022,#9023,#9024,#9025,#9026,#9027,#9028,#9029,
#9030));
#9119=CLOSED_SHELL('',(#9031,#9032,#9033,#9034));
#9120=CLOSED_SHELL('',(#9035,#9036,#9037,#9038));
#9121=CLOSED_SHELL('',(#9039,#9040,#9041,#9042,#9043,#9044,#9045));
#9122=CLOSED_SHELL('',(#9046,#9047,#9048,#9049,#9050,#9051,#9052,#9053,
#9054));
#9123=CLOSED_SHELL('',(#9055,#9056,#9057,#9058,#9059,#9060,#9061,#9062));
#9124=CLOSED_SHELL('',(#9063,#9064,#9065,#9066,#9067,#9068,#9069,#9070,
#9071,#9072,#9073,#9074));
#9125=DERIVED_UNIT_ELEMENT(#9207,1.);
#9126=DERIVED_UNIT_ELEMENT(#16801,-3.);
#9127=DERIVED_UNIT_ELEMENT(#9207,1.);
#9128=DERIVED_UNIT_ELEMENT(#16801,-3.);
#9129=DERIVED_UNIT_ELEMENT(#9207,1.);
#9130=DERIVED_UNIT_ELEMENT(#16801,-3.);
#9131=DERIVED_UNIT_ELEMENT(#9207,1.);
#9132=DERIVED_UNIT_ELEMENT(#16801,-3.);
#9133=DERIVED_UNIT_ELEMENT(#9207,1.);
#9134=DERIVED_UNIT_ELEMENT(#16801,-3.);
#9135=DERIVED_UNIT_ELEMENT(#9207,1.);
#9136=DERIVED_UNIT_ELEMENT(#16801,-3.);
#9137=DERIVED_UNIT_ELEMENT(#9207,1.);
#9138=DERIVED_UNIT_ELEMENT(#16801,-3.);
#9139=DERIVED_UNIT_ELEMENT(#9207,1.);
#9140=DERIVED_UNIT_ELEMENT(#16801,-3.);
#9141=DERIVED_UNIT_ELEMENT(#9207,1.);
#9142=DERIVED_UNIT_ELEMENT(#16801,-3.);
#9143=DERIVED_UNIT_ELEMENT(#9207,1.);
#9144=DERIVED_UNIT_ELEMENT(#16801,-3.);
#9145=DERIVED_UNIT_ELEMENT(#9207,1.);
#9146=DERIVED_UNIT_ELEMENT(#16801,-3.);
#9147=DERIVED_UNIT_ELEMENT(#9207,1.);
#9148=DERIVED_UNIT_ELEMENT(#16801,-3.);
#9149=DERIVED_UNIT_ELEMENT(#9207,1.);
#9150=DERIVED_UNIT_ELEMENT(#16801,-3.);
#9151=DERIVED_UNIT_ELEMENT(#9207,1.);
#9152=DERIVED_UNIT_ELEMENT(#16801,-3.);
#9153=DERIVED_UNIT_ELEMENT(#9207,1.);
#9154=DERIVED_UNIT_ELEMENT(#16801,-3.);
#9155=DERIVED_UNIT_ELEMENT(#9207,1.);
#9156=DERIVED_UNIT_ELEMENT(#16801,-3.);
#9157=DERIVED_UNIT_ELEMENT(#9207,1.);
#9158=DERIVED_UNIT_ELEMENT(#16801,-3.);
#9159=DERIVED_UNIT_ELEMENT(#9207,1.);
#9160=DERIVED_UNIT_ELEMENT(#16801,-3.);
#9161=DERIVED_UNIT_ELEMENT(#9207,1.);
#9162=DERIVED_UNIT_ELEMENT(#16801,-3.);
#9163=DERIVED_UNIT_ELEMENT(#9207,1.);
#9164=DERIVED_UNIT_ELEMENT(#16801,-3.);
#9165=DERIVED_UNIT_ELEMENT(#9207,1.);
#9166=DERIVED_UNIT_ELEMENT(#16801,-3.);
#9167=DERIVED_UNIT_ELEMENT(#9207,1.);
#9168=DERIVED_UNIT_ELEMENT(#16801,-3.);
#9169=DERIVED_UNIT_ELEMENT(#9207,1.);
#9170=DERIVED_UNIT_ELEMENT(#16801,-3.);
#9171=DERIVED_UNIT_ELEMENT(#9207,1.);
#9172=DERIVED_UNIT_ELEMENT(#16801,-3.);
#9173=DERIVED_UNIT_ELEMENT(#9207,1.);
#9174=DERIVED_UNIT_ELEMENT(#16801,-3.);
#9175=DERIVED_UNIT_ELEMENT(#9207,1.);
#9176=DERIVED_UNIT_ELEMENT(#16801,-3.);
#9177=DERIVED_UNIT_ELEMENT(#9207,1.);
#9178=DERIVED_UNIT_ELEMENT(#16801,-3.);
#9179=DERIVED_UNIT_ELEMENT(#9207,1.);
#9180=DERIVED_UNIT_ELEMENT(#16801,-3.);
#9181=DERIVED_UNIT_ELEMENT(#9207,1.);
#9182=DERIVED_UNIT_ELEMENT(#16801,-3.);
#9183=DERIVED_UNIT_ELEMENT(#9207,1.);
#9184=DERIVED_UNIT_ELEMENT(#16801,-3.);
#9185=DERIVED_UNIT_ELEMENT(#9207,1.);
#9186=DERIVED_UNIT_ELEMENT(#16801,-3.);
#9187=DERIVED_UNIT_ELEMENT(#9207,1.);
#9188=DERIVED_UNIT_ELEMENT(#16801,-3.);
#9189=DERIVED_UNIT_ELEMENT(#9207,1.);
#9190=DERIVED_UNIT_ELEMENT(#16801,-3.);
#9191=DERIVED_UNIT_ELEMENT(#9207,1.);
#9192=DERIVED_UNIT_ELEMENT(#16801,-3.);
#9193=DERIVED_UNIT_ELEMENT(#9207,1.);
#9194=DERIVED_UNIT_ELEMENT(#16801,-3.);
#9195=DERIVED_UNIT_ELEMENT(#9207,1.);
#9196=DERIVED_UNIT_ELEMENT(#16801,-3.);
#9197=DERIVED_UNIT_ELEMENT(#9207,1.);
#9198=DERIVED_UNIT_ELEMENT(#16801,-3.);
#9199=DERIVED_UNIT_ELEMENT(#9207,1.);
#9200=DERIVED_UNIT_ELEMENT(#16801,-3.);
#9201=DERIVED_UNIT_ELEMENT(#9207,1.);
#9202=DERIVED_UNIT_ELEMENT(#16801,-3.);
#9203=DERIVED_UNIT_ELEMENT(#9207,1.);
#9204=DERIVED_UNIT_ELEMENT(#16801,-3.);
#9205=DERIVED_UNIT_ELEMENT(#9207,1.);
#9206=DERIVED_UNIT_ELEMENT(#16801,-3.);
#9207=(
MASS_UNIT()
NAMED_UNIT(*)
SI_UNIT(.KILO.,.GRAM.)
);
#9208=DERIVED_UNIT((#9125,#9126));
#9209=DERIVED_UNIT((#9127,#9128));
#9210=DERIVED_UNIT((#9129,#9130));
#9211=DERIVED_UNIT((#9131,#9132));
#9212=DERIVED_UNIT((#9133,#9134));
#9213=DERIVED_UNIT((#9135,#9136));
#9214=DERIVED_UNIT((#9137,#9138));
#9215=DERIVED_UNIT((#9139,#9140));
#9216=DERIVED_UNIT((#9141,#9142));
#9217=DERIVED_UNIT((#9143,#9144));
#9218=DERIVED_UNIT((#9145,#9146));
#9219=DERIVED_UNIT((#9147,#9148));
#9220=DERIVED_UNIT((#9149,#9150));
#9221=DERIVED_UNIT((#9151,#9152));
#9222=DERIVED_UNIT((#9153,#9154));
#9223=DERIVED_UNIT((#9155,#9156));
#9224=DERIVED_UNIT((#9157,#9158));
#9225=DERIVED_UNIT((#9159,#9160));
#9226=DERIVED_UNIT((#9161,#9162));
#9227=DERIVED_UNIT((#9163,#9164));
#9228=DERIVED_UNIT((#9165,#9166));
#9229=DERIVED_UNIT((#9167,#9168));
#9230=DERIVED_UNIT((#9169,#9170));
#9231=DERIVED_UNIT((#9171,#9172));
#9232=DERIVED_UNIT((#9173,#9174));
#9233=DERIVED_UNIT((#9175,#9176));
#9234=DERIVED_UNIT((#9177,#9178));
#9235=DERIVED_UNIT((#9179,#9180));
#9236=DERIVED_UNIT((#9181,#9182));
#9237=DERIVED_UNIT((#9183,#9184));
#9238=DERIVED_UNIT((#9185,#9186));
#9239=DERIVED_UNIT((#9187,#9188));
#9240=DERIVED_UNIT((#9189,#9190));
#9241=DERIVED_UNIT((#9191,#9192));
#9242=DERIVED_UNIT((#9193,#9194));
#9243=DERIVED_UNIT((#9195,#9196));
#9244=DERIVED_UNIT((#9197,#9198));
#9245=DERIVED_UNIT((#9199,#9200));
#9246=DERIVED_UNIT((#9201,#9202));
#9247=DERIVED_UNIT((#9203,#9204));
#9248=DERIVED_UNIT((#9205,#9206));
#9249=MEASURE_REPRESENTATION_ITEM('density measure',
POSITIVE_RATIO_MEASURE(7850.),#9208);
#9250=MEASURE_REPRESENTATION_ITEM('density measure',
POSITIVE_RATIO_MEASURE(7850.),#9209);
#9251=MEASURE_REPRESENTATION_ITEM('density measure',
POSITIVE_RATIO_MEASURE(7850.),#9210);
#9252=MEASURE_REPRESENTATION_ITEM('density measure',
POSITIVE_RATIO_MEASURE(7850.),#9211);
#9253=MEASURE_REPRESENTATION_ITEM('density measure',
POSITIVE_RATIO_MEASURE(7850.),#9212);
#9254=MEASURE_REPRESENTATION_ITEM('density measure',
POSITIVE_RATIO_MEASURE(7850.),#9213);
#9255=MEASURE_REPRESENTATION_ITEM('density measure',
POSITIVE_RATIO_MEASURE(7850.),#9214);
#9256=MEASURE_REPRESENTATION_ITEM('density measure',
POSITIVE_RATIO_MEASURE(7850.),#9215);
#9257=MEASURE_REPRESENTATION_ITEM('density measure',
POSITIVE_RATIO_MEASURE(7850.),#9216);
#9258=MEASURE_REPRESENTATION_ITEM('density measure',
POSITIVE_RATIO_MEASURE(7850.),#9217);
#9259=MEASURE_REPRESENTATION_ITEM('density measure',
POSITIVE_RATIO_MEASURE(7850.),#9218);
#9260=MEASURE_REPRESENTATION_ITEM('density measure',
POSITIVE_RATIO_MEASURE(7850.),#9219);
#9261=MEASURE_REPRESENTATION_ITEM('density measure',
POSITIVE_RATIO_MEASURE(7850.),#9220);
#9262=MEASURE_REPRESENTATION_ITEM('density measure',
POSITIVE_RATIO_MEASURE(7850.),#9221);
#9263=MEASURE_REPRESENTATION_ITEM('density measure',
POSITIVE_RATIO_MEASURE(7850.),#9222);
#9264=MEASURE_REPRESENTATION_ITEM('density measure',
POSITIVE_RATIO_MEASURE(7850.),#9223);
#9265=MEASURE_REPRESENTATION_ITEM('density measure',
POSITIVE_RATIO_MEASURE(7850.),#9224);
#9266=MEASURE_REPRESENTATION_ITEM('density measure',
POSITIVE_RATIO_MEASURE(7850.),#9225);
#9267=MEASURE_REPRESENTATION_ITEM('density measure',
POSITIVE_RATIO_MEASURE(7850.),#9226);
#9268=MEASURE_REPRESENTATION_ITEM('density measure',
POSITIVE_RATIO_MEASURE(7850.),#9227);
#9269=MEASURE_REPRESENTATION_ITEM('density measure',
POSITIVE_RATIO_MEASURE(7850.),#9228);
#9270=MEASURE_REPRESENTATION_ITEM('density measure',
POSITIVE_RATIO_MEASURE(7850.),#9229);
#9271=MEASURE_REPRESENTATION_ITEM('density measure',
POSITIVE_RATIO_MEASURE(7850.),#9230);
#9272=MEASURE_REPRESENTATION_ITEM('density measure',
POSITIVE_RATIO_MEASURE(7850.),#9231);
#9273=MEASURE_REPRESENTATION_ITEM('density measure',
POSITIVE_RATIO_MEASURE(7850.),#9232);
#9274=MEASURE_REPRESENTATION_ITEM('density measure',
POSITIVE_RATIO_MEASURE(7850.),#9233);
#9275=MEASURE_REPRESENTATION_ITEM('density measure',
POSITIVE_RATIO_MEASURE(7850.),#9234);
#9276=MEASURE_REPRESENTATION_ITEM('density measure',
POSITIVE_RATIO_MEASURE(7850.),#9235);
#9277=MEASURE_REPRESENTATION_ITEM('density measure',
POSITIVE_RATIO_MEASURE(7850.),#9236);
#9278=MEASURE_REPRESENTATION_ITEM('density measure',
POSITIVE_RATIO_MEASURE(7850.),#9237);
#9279=MEASURE_REPRESENTATION_ITEM('density measure',
POSITIVE_RATIO_MEASURE(7850.),#9238);
#9280=MEASURE_REPRESENTATION_ITEM('density measure',
POSITIVE_RATIO_MEASURE(7850.),#9239);
#9281=MEASURE_REPRESENTATION_ITEM('density measure',
POSITIVE_RATIO_MEASURE(7850.),#9240);
#9282=MEASURE_REPRESENTATION_ITEM('density measure',
POSITIVE_RATIO_MEASURE(7850.),#9241);
#9283=MEASURE_REPRESENTATION_ITEM('density measure',
POSITIVE_RATIO_MEASURE(7850.),#9242);
#9284=MEASURE_REPRESENTATION_ITEM('density measure',
POSITIVE_RATIO_MEASURE(7850.),#9243);
#9285=MEASURE_REPRESENTATION_ITEM('density measure',
POSITIVE_RATIO_MEASURE(7850.),#9244);
#9286=MEASURE_REPRESENTATION_ITEM('density measure',
POSITIVE_RATIO_MEASURE(7850.),#9245);
#9287=MEASURE_REPRESENTATION_ITEM('density measure',
POSITIVE_RATIO_MEASURE(7850.),#9246);
#9288=MEASURE_REPRESENTATION_ITEM('density measure',
POSITIVE_RATIO_MEASURE(7850.),#9247);
#9289=MEASURE_REPRESENTATION_ITEM('density measure',
POSITIVE_RATIO_MEASURE(7850.),#9248);
#9290=PROPERTY_DEFINITION_REPRESENTATION(#9495,#9372);
#9291=PROPERTY_DEFINITION_REPRESENTATION(#9496,#9373);
#9292=PROPERTY_DEFINITION_REPRESENTATION(#9497,#9374);
#9293=PROPERTY_DEFINITION_REPRESENTATION(#9498,#9375);
#9294=PROPERTY_DEFINITION_REPRESENTATION(#9499,#9376);
#9295=PROPERTY_DEFINITION_REPRESENTATION(#9500,#9377);
#9296=PROPERTY_DEFINITION_REPRESENTATION(#9501,#9378);
#9297=PROPERTY_DEFINITION_REPRESENTATION(#9502,#9379);
#9298=PROPERTY_DEFINITION_REPRESENTATION(#9503,#9380);
#9299=PROPERTY_DEFINITION_REPRESENTATION(#9504,#9381);
#9300=PROPERTY_DEFINITION_REPRESENTATION(#9505,#9382);
#9301=PROPERTY_DEFINITION_REPRESENTATION(#9506,#9383);
#9302=PROPERTY_DEFINITION_REPRESENTATION(#9507,#9384);
#9303=PROPERTY_DEFINITION_REPRESENTATION(#9508,#9385);
#9304=PROPERTY_DEFINITION_REPRESENTATION(#9509,#9386);
#9305=PROPERTY_DEFINITION_REPRESENTATION(#9510,#9387);
#9306=PROPERTY_DEFINITION_REPRESENTATION(#9511,#9388);
#9307=PROPERTY_DEFINITION_REPRESENTATION(#9512,#9389);
#9308=PROPERTY_DEFINITION_REPRESENTATION(#9513,#9390);
#9309=PROPERTY_DEFINITION_REPRESENTATION(#9514,#9391);
#9310=PROPERTY_DEFINITION_REPRESENTATION(#9515,#9392);
#9311=PROPERTY_DEFINITION_REPRESENTATION(#9516,#9393);
#9312=PROPERTY_DEFINITION_REPRESENTATION(#9517,#9394);
#9313=PROPERTY_DEFINITION_REPRESENTATION(#9518,#9395);
#9314=PROPERTY_DEFINITION_REPRESENTATION(#9519,#9396);
#9315=PROPERTY_DEFINITION_REPRESENTATION(#9520,#9397);
#9316=PROPERTY_DEFINITION_REPRESENTATION(#9521,#9398);
#9317=PROPERTY_DEFINITION_REPRESENTATION(#9522,#9399);
#9318=PROPERTY_DEFINITION_REPRESENTATION(#9523,#9400);
#9319=PROPERTY_DEFINITION_REPRESENTATION(#9524,#9401);
#9320=PROPERTY_DEFINITION_REPRESENTATION(#9525,#9402);
#9321=PROPERTY_DEFINITION_REPRESENTATION(#9526,#9403);
#9322=PROPERTY_DEFINITION_REPRESENTATION(#9527,#9404);
#9323=PROPERTY_DEFINITION_REPRESENTATION(#9528,#9405);
#9324=PROPERTY_DEFINITION_REPRESENTATION(#9529,#9406);
#9325=PROPERTY_DEFINITION_REPRESENTATION(#9530,#9407);
#9326=PROPERTY_DEFINITION_REPRESENTATION(#9531,#9408);
#9327=PROPERTY_DEFINITION_REPRESENTATION(#9532,#9409);
#9328=PROPERTY_DEFINITION_REPRESENTATION(#9533,#9410);
#9329=PROPERTY_DEFINITION_REPRESENTATION(#9534,#9411);
#9330=PROPERTY_DEFINITION_REPRESENTATION(#9535,#9412);
#9331=PROPERTY_DEFINITION_REPRESENTATION(#9536,#9413);
#9332=PROPERTY_DEFINITION_REPRESENTATION(#9537,#9414);
#9333=PROPERTY_DEFINITION_REPRESENTATION(#9538,#9415);
#9334=PROPERTY_DEFINITION_REPRESENTATION(#9539,#9416);
#9335=PROPERTY_DEFINITION_REPRESENTATION(#9540,#9417);
#9336=PROPERTY_DEFINITION_REPRESENTATION(#9541,#9418);
#9337=PROPERTY_DEFINITION_REPRESENTATION(#9542,#9419);
#9338=PROPERTY_DEFINITION_REPRESENTATION(#9543,#9420);
#9339=PROPERTY_DEFINITION_REPRESENTATION(#9544,#9421);
#9340=PROPERTY_DEFINITION_REPRESENTATION(#9545,#9422);
#9341=PROPERTY_DEFINITION_REPRESENTATION(#9546,#9423);
#9342=PROPERTY_DEFINITION_REPRESENTATION(#9547,#9424);
#9343=PROPERTY_DEFINITION_REPRESENTATION(#9548,#9425);
#9344=PROPERTY_DEFINITION_REPRESENTATION(#9549,#9426);
#9345=PROPERTY_DEFINITION_REPRESENTATION(#9550,#9427);
#9346=PROPERTY_DEFINITION_REPRESENTATION(#9551,#9428);
#9347=PROPERTY_DEFINITION_REPRESENTATION(#9552,#9429);
#9348=PROPERTY_DEFINITION_REPRESENTATION(#9553,#9430);
#9349=PROPERTY_DEFINITION_REPRESENTATION(#9554,#9431);
#9350=PROPERTY_DEFINITION_REPRESENTATION(#9555,#9432);
#9351=PROPERTY_DEFINITION_REPRESENTATION(#9556,#9433);
#9352=PROPERTY_DEFINITION_REPRESENTATION(#9557,#9434);
#9353=PROPERTY_DEFINITION_REPRESENTATION(#9558,#9435);
#9354=PROPERTY_DEFINITION_REPRESENTATION(#9559,#9436);
#9355=PROPERTY_DEFINITION_REPRESENTATION(#9560,#9437);
#9356=PROPERTY_DEFINITION_REPRESENTATION(#9561,#9438);
#9357=PROPERTY_DEFINITION_REPRESENTATION(#9562,#9439);
#9358=PROPERTY_DEFINITION_REPRESENTATION(#9563,#9440);
#9359=PROPERTY_DEFINITION_REPRESENTATION(#9564,#9441);
#9360=PROPERTY_DEFINITION_REPRESENTATION(#9565,#9442);
#9361=PROPERTY_DEFINITION_REPRESENTATION(#9566,#9443);
#9362=PROPERTY_DEFINITION_REPRESENTATION(#9567,#9444);
#9363=PROPERTY_DEFINITION_REPRESENTATION(#9568,#9445);
#9364=PROPERTY_DEFINITION_REPRESENTATION(#9569,#9446);
#9365=PROPERTY_DEFINITION_REPRESENTATION(#9570,#9447);
#9366=PROPERTY_DEFINITION_REPRESENTATION(#9571,#9448);
#9367=PROPERTY_DEFINITION_REPRESENTATION(#9572,#9449);
#9368=PROPERTY_DEFINITION_REPRESENTATION(#9573,#9450);
#9369=PROPERTY_DEFINITION_REPRESENTATION(#9574,#9451);
#9370=PROPERTY_DEFINITION_REPRESENTATION(#9575,#9452);
#9371=PROPERTY_DEFINITION_REPRESENTATION(#9576,#9453);
#9372=REPRESENTATION('material name',(#9454),#16753);
#9373=REPRESENTATION('density',(#9249),#16753);
#9374=REPRESENTATION('material name',(#9455),#16754);
#9375=REPRESENTATION('density',(#9250),#16754);
#9376=REPRESENTATION('material name',(#9456),#16755);
#9377=REPRESENTATION('density',(#9251),#16755);
#9378=REPRESENTATION('material name',(#9457),#16756);
#9379=REPRESENTATION('density',(#9252),#16756);
#9380=REPRESENTATION('material name',(#9458),#16757);
#9381=REPRESENTATION('density',(#9253),#16757);
#9382=REPRESENTATION('material name',(#9459),#16758);
#9383=REPRESENTATION('density',(#9254),#16758);
#9384=REPRESENTATION('material name',(#9460),#16759);
#9385=REPRESENTATION('density',(#9255),#16759);
#9386=REPRESENTATION('material name',(#9461),#16760);
#9387=REPRESENTATION('density',(#9256),#16760);
#9388=REPRESENTATION('material name',(#9462),#16761);
#9389=REPRESENTATION('density',(#9257),#16761);
#9390=REPRESENTATION('material name',(#9463),#16762);
#9391=REPRESENTATION('density',(#9258),#16762);
#9392=REPRESENTATION('material name',(#9464),#16763);
#9393=REPRESENTATION('density',(#9259),#16763);
#9394=REPRESENTATION('material name',(#9465),#16764);
#9395=REPRESENTATION('density',(#9260),#16764);
#9396=REPRESENTATION('material name',(#9466),#16765);
#9397=REPRESENTATION('density',(#9261),#16765);
#9398=REPRESENTATION('material name',(#9467),#16766);
#9399=REPRESENTATION('density',(#9262),#16766);
#9400=REPRESENTATION('material name',(#9468),#16768);
#9401=REPRESENTATION('density',(#9263),#16768);
#9402=REPRESENTATION('material name',(#9469),#16769);
#9403=REPRESENTATION('density',(#9264),#16769);
#9404=REPRESENTATION('material name',(#9470),#16770);
#9405=REPRESENTATION('density',(#9265),#16770);
#9406=REPRESENTATION('material name',(#9471),#16771);
#9407=REPRESENTATION('density',(#9266),#16771);
#9408=REPRESENTATION('material name',(#9472),#16772);
#9409=REPRESENTATION('density',(#9267),#16772);
#9410=REPRESENTATION('material name',(#9473),#16774);
#9411=REPRESENTATION('density',(#9268),#16774);
#9412=REPRESENTATION('material name',(#9474),#16775);
#9413=REPRESENTATION('density',(#9269),#16775);
#9414=REPRESENTATION('material name',(#9475),#16776);
#9415=REPRESENTATION('density',(#9270),#16776);
#9416=REPRESENTATION('material name',(#9476),#16777);
#9417=REPRESENTATION('density',(#9271),#16777);
#9418=REPRESENTATION('material name',(#9477),#16778);
#9419=REPRESENTATION('density',(#9272),#16778);
#9420=REPRESENTATION('material name',(#9478),#16780);
#9421=REPRESENTATION('density',(#9273),#16780);
#9422=REPRESENTATION('material name',(#9479),#16781);
#9423=REPRESENTATION('density',(#9274),#16781);
#9424=REPRESENTATION('material name',(#9480),#16782);
#9425=REPRESENTATION('density',(#9275),#16782);
#9426=REPRESENTATION('material name',(#9481),#16783);
#9427=REPRESENTATION('density',(#9276),#16783);
#9428=REPRESENTATION('material name',(#9482),#16784);
#9429=REPRESENTATION('density',(#9277),#16784);
#9430=REPRESENTATION('material name',(#9483),#16786);
#9431=REPRESENTATION('density',(#9278),#16786);
#9432=REPRESENTATION('material name',(#9484),#16787);
#9433=REPRESENTATION('density',(#9279),#16787);
#9434=REPRESENTATION('material name',(#9485),#16788);
#9435=REPRESENTATION('density',(#9280),#16788);
#9436=REPRESENTATION('material name',(#9486),#16790);
#9437=REPRESENTATION('density',(#9281),#16790);
#9438=REPRESENTATION('material name',(#9487),#16791);
#9439=REPRESENTATION('density',(#9282),#16791);
#9440=REPRESENTATION('material name',(#9488),#16792);
#9441=REPRESENTATION('density',(#9283),#16792);
#9442=REPRESENTATION('material name',(#9489),#16793);
#9443=REPRESENTATION('density',(#9284),#16793);
#9444=REPRESENTATION('material name',(#9490),#16794);
#9445=REPRESENTATION('density',(#9285),#16794);
#9446=REPRESENTATION('material name',(#9491),#16795);
#9447=REPRESENTATION('density',(#9286),#16795);
#9448=REPRESENTATION('material name',(#9492),#16796);
#9449=REPRESENTATION('density',(#9287),#16796);
#9450=REPRESENTATION('material name',(#9493),#16797);
#9451=REPRESENTATION('density',(#9288),#16797);
#9452=REPRESENTATION('material name',(#9494),#16798);
#9453=REPRESENTATION('density',(#9289),#16798);
#9454=DESCRIPTIVE_REPRESENTATION_ITEM('Steel','Steel');
#9455=DESCRIPTIVE_REPRESENTATION_ITEM('Steel','Steel');
#9456=DESCRIPTIVE_REPRESENTATION_ITEM('Steel','Steel');
#9457=DESCRIPTIVE_REPRESENTATION_ITEM('Steel','Steel');
#9458=DESCRIPTIVE_REPRESENTATION_ITEM('Steel','Steel');
#9459=DESCRIPTIVE_REPRESENTATION_ITEM('Steel','Steel');
#9460=DESCRIPTIVE_REPRESENTATION_ITEM('Steel','Steel');
#9461=DESCRIPTIVE_REPRESENTATION_ITEM('Steel','Steel');
#9462=DESCRIPTIVE_REPRESENTATION_ITEM('Steel','Steel');
#9463=DESCRIPTIVE_REPRESENTATION_ITEM('Steel','Steel');
#9464=DESCRIPTIVE_REPRESENTATION_ITEM('Steel','Steel');
#9465=DESCRIPTIVE_REPRESENTATION_ITEM('Steel','Steel');
#9466=DESCRIPTIVE_REPRESENTATION_ITEM('Steel','Steel');
#9467=DESCRIPTIVE_REPRESENTATION_ITEM('Steel','Steel');
#9468=DESCRIPTIVE_REPRESENTATION_ITEM('Steel','Steel');
#9469=DESCRIPTIVE_REPRESENTATION_ITEM('Steel','Steel');
#9470=DESCRIPTIVE_REPRESENTATION_ITEM('Steel','Steel');
#9471=DESCRIPTIVE_REPRESENTATION_ITEM('Steel','Steel');
#9472=DESCRIPTIVE_REPRESENTATION_ITEM('Steel','Steel');
#9473=DESCRIPTIVE_REPRESENTATION_ITEM('Steel','Steel');
#9474=DESCRIPTIVE_REPRESENTATION_ITEM('Steel','Steel');
#9475=DESCRIPTIVE_REPRESENTATION_ITEM('Steel','Steel');
#9476=DESCRIPTIVE_REPRESENTATION_ITEM('Steel','Steel');
#9477=DESCRIPTIVE_REPRESENTATION_ITEM('Steel','Steel');
#9478=DESCRIPTIVE_REPRESENTATION_ITEM('Steel','Steel');
#9479=DESCRIPTIVE_REPRESENTATION_ITEM('Steel','Steel');
#9480=DESCRIPTIVE_REPRESENTATION_ITEM('Steel','Steel');
#9481=DESCRIPTIVE_REPRESENTATION_ITEM('Steel','Steel');
#9482=DESCRIPTIVE_REPRESENTATION_ITEM('Steel','Steel');
#9483=DESCRIPTIVE_REPRESENTATION_ITEM('Steel','Steel');
#9484=DESCRIPTIVE_REPRESENTATION_ITEM('Steel','Steel');
#9485=DESCRIPTIVE_REPRESENTATION_ITEM('Steel','Steel');
#9486=DESCRIPTIVE_REPRESENTATION_ITEM('Steel','Steel');
#9487=DESCRIPTIVE_REPRESENTATION_ITEM('Steel','Steel');
#9488=DESCRIPTIVE_REPRESENTATION_ITEM('Steel','Steel');
#9489=DESCRIPTIVE_REPRESENTATION_ITEM('Steel','Steel');
#9490=DESCRIPTIVE_REPRESENTATION_ITEM('Steel','Steel');
#9491=DESCRIPTIVE_REPRESENTATION_ITEM('Steel','Steel');
#9492=DESCRIPTIVE_REPRESENTATION_ITEM('Steel','Steel');
#9493=DESCRIPTIVE_REPRESENTATION_ITEM('Steel','Steel');
#9494=DESCRIPTIVE_REPRESENTATION_ITEM('Steel','Steel');
#9495=PROPERTY_DEFINITION('material property','material name',#17064);
#9496=PROPERTY_DEFINITION('material property','density of part',#17064);
#9497=PROPERTY_DEFINITION('material property','material name',#17065);
#9498=PROPERTY_DEFINITION('material property','density of part',#17065);
#9499=PROPERTY_DEFINITION('material property','material name',#17066);
#9500=PROPERTY_DEFINITION('material property','density of part',#17066);
#9501=PROPERTY_DEFINITION('material property','material name',#17067);
#9502=PROPERTY_DEFINITION('material property','density of part',#17067);
#9503=PROPERTY_DEFINITION('material property','material name',#17068);
#9504=PROPERTY_DEFINITION('material property','density of part',#17068);
#9505=PROPERTY_DEFINITION('material property','material name',#17069);
#9506=PROPERTY_DEFINITION('material property','density of part',#17069);
#9507=PROPERTY_DEFINITION('material property','material name',#17070);
#9508=PROPERTY_DEFINITION('material property','density of part',#17070);
#9509=PROPERTY_DEFINITION('material property','material name',#17071);
#9510=PROPERTY_DEFINITION('material property','density of part',#17071);
#9511=PROPERTY_DEFINITION('material property','material name',#17072);
#9512=PROPERTY_DEFINITION('material property','density of part',#17072);
#9513=PROPERTY_DEFINITION('material property','material name',#17073);
#9514=PROPERTY_DEFINITION('material property','density of part',#17073);
#9515=PROPERTY_DEFINITION('material property','material name',#17074);
#9516=PROPERTY_DEFINITION('material property','density of part',#17074);
#9517=PROPERTY_DEFINITION('material property','material name',#17075);
#9518=PROPERTY_DEFINITION('material property','density of part',#17075);
#9519=PROPERTY_DEFINITION('material property','material name',#17076);
#9520=PROPERTY_DEFINITION('material property','density of part',#17076);
#9521=PROPERTY_DEFINITION('material property','material name',#17077);
#9522=PROPERTY_DEFINITION('material property','density of part',#17077);
#9523=PROPERTY_DEFINITION('material property','material name',#17079);
#9524=PROPERTY_DEFINITION('material property','density of part',#17079);
#9525=PROPERTY_DEFINITION('material property','material name',#17080);
#9526=PROPERTY_DEFINITION('material property','density of part',#17080);
#9527=PROPERTY_DEFINITION('material property','material name',#17081);
#9528=PROPERTY_DEFINITION('material property','density of part',#17081);
#9529=PROPERTY_DEFINITION('material property','material name',#17082);
#9530=PROPERTY_DEFINITION('material property','density of part',#17082);
#9531=PROPERTY_DEFINITION('material property','material name',#17083);
#9532=PROPERTY_DEFINITION('material property','density of part',#17083);
#9533=PROPERTY_DEFINITION('material property','material name',#17085);
#9534=PROPERTY_DEFINITION('material property','density of part',#17085);
#9535=PROPERTY_DEFINITION('material property','material name',#17086);
#9536=PROPERTY_DEFINITION('material property','density of part',#17086);
#9537=PROPERTY_DEFINITION('material property','material name',#17087);
#9538=PROPERTY_DEFINITION('material property','density of part',#17087);
#9539=PROPERTY_DEFINITION('material property','material name',#17088);
#9540=PROPERTY_DEFINITION('material property','density of part',#17088);
#9541=PROPERTY_DEFINITION('material property','material name',#17089);
#9542=PROPERTY_DEFINITION('material property','density of part',#17089);
#9543=PROPERTY_DEFINITION('material property','material name',#17091);
#9544=PROPERTY_DEFINITION('material property','density of part',#17091);
#9545=PROPERTY_DEFINITION('material property','material name',#17092);
#9546=PROPERTY_DEFINITION('material property','density of part',#17092);
#9547=PROPERTY_DEFINITION('material property','material name',#17093);
#9548=PROPERTY_DEFINITION('material property','density of part',#17093);
#9549=PROPERTY_DEFINITION('material property','material name',#17094);
#9550=PROPERTY_DEFINITION('material property','density of part',#17094);
#9551=PROPERTY_DEFINITION('material property','material name',#17095);
#9552=PROPERTY_DEFINITION('material property','density of part',#17095);
#9553=PROPERTY_DEFINITION('material property','material name',#17097);
#9554=PROPERTY_DEFINITION('material property','density of part',#17097);
#9555=PROPERTY_DEFINITION('material property','material name',#17098);
#9556=PROPERTY_DEFINITION('material property','density of part',#17098);
#9557=PROPERTY_DEFINITION('material property','material name',#17099);
#9558=PROPERTY_DEFINITION('material property','density of part',#17099);
#9559=PROPERTY_DEFINITION('material property','material name',#17101);
#9560=PROPERTY_DEFINITION('material property','density of part',#17101);
#9561=PROPERTY_DEFINITION('material property','material name',#17102);
#9562=PROPERTY_DEFINITION('material property','density of part',#17102);
#9563=PROPERTY_DEFINITION('material property','material name',#17103);
#9564=PROPERTY_DEFINITION('material property','density of part',#17103);
#9565=PROPERTY_DEFINITION('material property','material name',#17104);
#9566=PROPERTY_DEFINITION('material property','density of part',#17104);
#9567=PROPERTY_DEFINITION('material property','material name',#17105);
#9568=PROPERTY_DEFINITION('material property','density of part',#17105);
#9569=PROPERTY_DEFINITION('material property','material name',#17106);
#9570=PROPERTY_DEFINITION('material property','density of part',#17106);
#9571=PROPERTY_DEFINITION('material property','material name',#17107);
#9572=PROPERTY_DEFINITION('material property','density of part',#17107);
#9573=PROPERTY_DEFINITION('material property','material name',#17108);
#9574=PROPERTY_DEFINITION('material property','density of part',#17108);
#9575=PROPERTY_DEFINITION('material property','material name',#17109);
#9576=PROPERTY_DEFINITION('material property','density of part',#17109);
#9577=AXIS2_PLACEMENT_3D('',#13675,#10752,#10753);
#9578=AXIS2_PLACEMENT_3D('',#13676,#10754,#10755);
#9579=AXIS2_PLACEMENT_3D('',#13677,#10756,#10757);
#9580=AXIS2_PLACEMENT_3D('',#13678,#10758,#10759);
#9581=AXIS2_PLACEMENT_3D('',#13680,#10760,#10761);
#9582=AXIS2_PLACEMENT_3D('',#13683,#10763,#10764);
#9583=AXIS2_PLACEMENT_3D('',#13684,#10765,#10766);
#9584=AXIS2_PLACEMENT_3D('',#13686,#10767,#10768);
#9585=AXIS2_PLACEMENT_3D('',#13689,#10770,#10771);
#9586=AXIS2_PLACEMENT_3D('',#13690,#10772,#10773);
#9587=AXIS2_PLACEMENT_3D('',#13692,#10774,#10775);
#9588=AXIS2_PLACEMENT_3D('',#13695,#10777,#10778);
#9589=AXIS2_PLACEMENT_3D('',#13696,#10779,#10780);
#9590=AXIS2_PLACEMENT_3D('',#13698,#10781,#10782);
#9591=AXIS2_PLACEMENT_3D('',#13701,#10784,#10785);
#9592=AXIS2_PLACEMENT_3D('',#13702,#10786,#10787);
#9593=AXIS2_PLACEMENT_3D('',#13704,#10788,#10789);
#9594=AXIS2_PLACEMENT_3D('',#13707,#10791,#10792);
#9595=AXIS2_PLACEMENT_3D('',#13708,#10793,#10794);
#9596=AXIS2_PLACEMENT_3D('',#13710,#10795,#10796);
#9597=AXIS2_PLACEMENT_3D('',#13713,#10798,#10799);
#9598=AXIS2_PLACEMENT_3D('',#13714,#10800,#10801);
#9599=AXIS2_PLACEMENT_3D('',#13716,#10802,#10803);
#9600=AXIS2_PLACEMENT_3D('',#13719,#10805,#10806);
#9601=AXIS2_PLACEMENT_3D('',#13720,#10807,#10808);
#9602=AXIS2_PLACEMENT_3D('',#13722,#10809,#10810);
#9603=AXIS2_PLACEMENT_3D('',#13725,#10812,#10813);
#9604=AXIS2_PLACEMENT_3D('',#13726,#10814,#10815);
#9605=AXIS2_PLACEMENT_3D('',#13728,#10816,#10817);
#9606=AXIS2_PLACEMENT_3D('',#13731,#10819,#10820);
#9607=AXIS2_PLACEMENT_3D('',#13732,#10821,#10822);
#9608=AXIS2_PLACEMENT_3D('',#13734,#10823,#10824);
#9609=AXIS2_PLACEMENT_3D('',#13737,#10826,#10827);
#9610=AXIS2_PLACEMENT_3D('',#13738,#10828,#10829);
#9611=AXIS2_PLACEMENT_3D('',#13740,#10830,#10831);
#9612=AXIS2_PLACEMENT_3D('',#13743,#10833,#10834);
#9613=AXIS2_PLACEMENT_3D('',#13744,#10835,#10836);
#9614=AXIS2_PLACEMENT_3D('',#13746,#10837,#10838);
#9615=AXIS2_PLACEMENT_3D('',#13749,#10840,#10841);
#9616=AXIS2_PLACEMENT_3D('',#13750,#10842,#10843);
#9617=AXIS2_PLACEMENT_3D('',#13759,#10848,#10849);
#9618=AXIS2_PLACEMENT_3D('',#13765,#10853,#10854);
#9619=AXIS2_PLACEMENT_3D('',#13771,#10858,#10859);
#9620=AXIS2_PLACEMENT_3D('',#13774,#10862,#10863);
#9621=AXIS2_PLACEMENT_3D('',#13775,#10864,#10865);
#9622=AXIS2_PLACEMENT_3D('',#13776,#10866,#10867);
#9623=AXIS2_PLACEMENT_3D('',#13777,#10868,#10869);
#9624=AXIS2_PLACEMENT_3D('',#13786,#10874,#10875);
#9625=AXIS2_PLACEMENT_3D('',#13792,#10879,#10880);
#9626=AXIS2_PLACEMENT_3D('',#13798,#10884,#10885);
#9627=AXIS2_PLACEMENT_3D('',#13801,#10888,#10889);
#9628=AXIS2_PLACEMENT_3D('',#13802,#10890,#10891);
#9629=AXIS2_PLACEMENT_3D('',#13803,#10892,#10893);
#9630=AXIS2_PLACEMENT_3D('',#13804,#10894,#10895);
#9631=AXIS2_PLACEMENT_3D('',#13813,#10900,#10901);
#9632=AXIS2_PLACEMENT_3D('',#13819,#10905,#10906);
#9633=AXIS2_PLACEMENT_3D('',#13825,#10910,#10911);
#9634=AXIS2_PLACEMENT_3D('',#13828,#10914,#10915);
#9635=AXIS2_PLACEMENT_3D('',#13829,#10916,#10917);
#9636=AXIS2_PLACEMENT_3D('',#13830,#10918,#10919);
#9637=AXIS2_PLACEMENT_3D('',#13831,#10920,#10921);
#9638=AXIS2_PLACEMENT_3D('',#13836,#10923,#10924);
#9639=AXIS2_PLACEMENT_3D('',#13839,#10926,#10927);
#9640=AXIS2_PLACEMENT_3D('',#13840,#10928,#10929);
#9641=AXIS2_PLACEMENT_3D('',#13845,#10931,#10932);
#9642=AXIS2_PLACEMENT_3D('',#13848,#10934,#10935);
#9643=AXIS2_PLACEMENT_3D('',#13849,#10936,#10937);
#9644=AXIS2_PLACEMENT_3D('',#13853,#10939,#10940);
#9645=AXIS2_PLACEMENT_3D('',#13854,#10941,#10942);
#9646=AXIS2_PLACEMENT_3D('',#13864,#10943,#10944);
#9647=AXIS2_PLACEMENT_3D('',#13886,#10946,#10947);
#9648=AXIS2_PLACEMENT_3D('',#13887,#10948,#10949);
#9649=AXIS2_PLACEMENT_3D('',#13889,#10951,#10952);
#9650=AXIS2_PLACEMENT_3D('',#13890,#10953,#10954);
#9651=AXIS2_PLACEMENT_3D('',#13892,#10956,#10957);
#9652=AXIS2_PLACEMENT_3D('',#13893,#10958,#10959);
#9653=AXIS2_PLACEMENT_3D('',#13895,#10960,#10961);
#9654=AXIS2_PLACEMENT_3D('',#13896,#10962,#10963);
#9655=AXIS2_PLACEMENT_3D('',#13897,#10964,#10965);
#9656=AXIS2_PLACEMENT_3D('',#13899,#10967,#10968);
#9657=AXIS2_PLACEMENT_3D('',#13900,#10969,#10970);
#9658=AXIS2_PLACEMENT_3D('',#13902,#10971,#10972);
#9659=AXIS2_PLACEMENT_3D('',#13903,#10973,#10974);
#9660=AXIS2_PLACEMENT_3D('',#13914,#10981,#10982);
#9661=AXIS2_PLACEMENT_3D('',#13916,#10983,#10984);
#9662=AXIS2_PLACEMENT_3D('',#13918,#10986,#10987);
#9663=AXIS2_PLACEMENT_3D('',#13920,#10988,#10989);
#9664=AXIS2_PLACEMENT_3D('',#13922,#10991,#10992);
#9665=AXIS2_PLACEMENT_3D('',#13924,#10993,#10994);
#9666=AXIS2_PLACEMENT_3D('',#13928,#10997,#10998);
#9667=AXIS2_PLACEMENT_3D('',#13929,#10999,#11000);
#9668=AXIS2_PLACEMENT_3D('',#13935,#11004,#11005);
#9669=AXIS2_PLACEMENT_3D('',#13939,#11008,#11009);
#9670=AXIS2_PLACEMENT_3D('',#13943,#11012,#11013);
#9671=AXIS2_PLACEMENT_3D('',#13945,#11015,#11016);
#9672=AXIS2_PLACEMENT_3D('',#13946,#11017,#11018);
#9673=AXIS2_PLACEMENT_3D('',#13947,#11019,#11020);
#9674=AXIS2_PLACEMENT_3D('',#13952,#11022,#11023);
#9675=AXIS2_PLACEMENT_3D('',#13955,#11025,#11026);
#9676=AXIS2_PLACEMENT_3D('',#13956,#11027,#11028);
#9677=AXIS2_PLACEMENT_3D('',#13961,#11030,#11031);
#9678=AXIS2_PLACEMENT_3D('',#13964,#11033,#11034);
#9679=AXIS2_PLACEMENT_3D('',#13965,#11035,#11036);
#9680=AXIS2_PLACEMENT_3D('',#13969,#11038,#11039);
#9681=AXIS2_PLACEMENT_3D('',#13970,#11040,#11041);
#9682=AXIS2_PLACEMENT_3D('',#13980,#11042,#11043);
#9683=AXIS2_PLACEMENT_3D('',#14002,#11045,#11046);
#9684=AXIS2_PLACEMENT_3D('',#14003,#11047,#11048);
#9685=AXIS2_PLACEMENT_3D('',#14005,#11050,#11051);
#9686=AXIS2_PLACEMENT_3D('',#14006,#11052,#11053);
#9687=AXIS2_PLACEMENT_3D('',#14008,#11055,#11056);
#9688=AXIS2_PLACEMENT_3D('',#14009,#11057,#11058);
#9689=AXIS2_PLACEMENT_3D('',#14011,#11059,#11060);
#9690=AXIS2_PLACEMENT_3D('',#14012,#11061,#11062);
#9691=AXIS2_PLACEMENT_3D('',#14013,#11063,#11064);
#9692=AXIS2_PLACEMENT_3D('',#14015,#11066,#11067);
#9693=AXIS2_PLACEMENT_3D('',#14016,#11068,#11069);
#9694=AXIS2_PLACEMENT_3D('',#14018,#11070,#11071);
#9695=AXIS2_PLACEMENT_3D('',#14019,#11072,#11073);
#9696=AXIS2_PLACEMENT_3D('',#14030,#11080,#11081);
#9697=AXIS2_PLACEMENT_3D('',#14032,#11082,#11083);
#9698=AXIS2_PLACEMENT_3D('',#14034,#11085,#11086);
#9699=AXIS2_PLACEMENT_3D('',#14036,#11087,#11088);
#9700=AXIS2_PLACEMENT_3D('',#14038,#11090,#11091);
#9701=AXIS2_PLACEMENT_3D('',#14040,#11092,#11093);
#9702=AXIS2_PLACEMENT_3D('',#14044,#11096,#11097);
#9703=AXIS2_PLACEMENT_3D('',#14045,#11098,#11099);
#9704=AXIS2_PLACEMENT_3D('',#14051,#11103,#11104);
#9705=AXIS2_PLACEMENT_3D('',#14055,#11107,#11108);
#9706=AXIS2_PLACEMENT_3D('',#14059,#11111,#11112);
#9707=AXIS2_PLACEMENT_3D('',#14061,#11114,#11115);
#9708=AXIS2_PLACEMENT_3D('',#14062,#11116,#11117);
#9709=AXIS2_PLACEMENT_3D('',#14063,#11118,#11119);
#9710=AXIS2_PLACEMENT_3D('',#14068,#11121,#11122);
#9711=AXIS2_PLACEMENT_3D('',#14071,#11124,#11125);
#9712=AXIS2_PLACEMENT_3D('',#14072,#11126,#11127);
#9713=AXIS2_PLACEMENT_3D('',#14077,#11129,#11130);
#9714=AXIS2_PLACEMENT_3D('',#14080,#11132,#11133);
#9715=AXIS2_PLACEMENT_3D('',#14081,#11134,#11135);
#9716=AXIS2_PLACEMENT_3D('',#14085,#11137,#11138);
#9717=AXIS2_PLACEMENT_3D('',#14086,#11139,#11140);
#9718=AXIS2_PLACEMENT_3D('',#14096,#11141,#11142);
#9719=AXIS2_PLACEMENT_3D('',#14118,#11144,#11145);
#9720=AXIS2_PLACEMENT_3D('',#14119,#11146,#11147);
#9721=AXIS2_PLACEMENT_3D('',#14121,#11149,#11150);
#9722=AXIS2_PLACEMENT_3D('',#14122,#11151,#11152);
#9723=AXIS2_PLACEMENT_3D('',#14124,#11154,#11155);
#9724=AXIS2_PLACEMENT_3D('',#14125,#11156,#11157);
#9725=AXIS2_PLACEMENT_3D('',#14127,#11158,#11159);
#9726=AXIS2_PLACEMENT_3D('',#14128,#11160,#11161);
#9727=AXIS2_PLACEMENT_3D('',#14129,#11162,#11163);
#9728=AXIS2_PLACEMENT_3D('',#14131,#11165,#11166);
#9729=AXIS2_PLACEMENT_3D('',#14132,#11167,#11168);
#9730=AXIS2_PLACEMENT_3D('',#14134,#11169,#11170);
#9731=AXIS2_PLACEMENT_3D('',#14135,#11171,#11172);
#9732=AXIS2_PLACEMENT_3D('',#14146,#11179,#11180);
#9733=AXIS2_PLACEMENT_3D('',#14148,#11181,#11182);
#9734=AXIS2_PLACEMENT_3D('',#14150,#11184,#11185);
#9735=AXIS2_PLACEMENT_3D('',#14152,#11186,#11187);
#9736=AXIS2_PLACEMENT_3D('',#14154,#11189,#11190);
#9737=AXIS2_PLACEMENT_3D('',#14156,#11191,#11192);
#9738=AXIS2_PLACEMENT_3D('',#14160,#11195,#11196);
#9739=AXIS2_PLACEMENT_3D('',#14161,#11197,#11198);
#9740=AXIS2_PLACEMENT_3D('',#14167,#11202,#11203);
#9741=AXIS2_PLACEMENT_3D('',#14171,#11206,#11207);
#9742=AXIS2_PLACEMENT_3D('',#14175,#11210,#11211);
#9743=AXIS2_PLACEMENT_3D('',#14177,#11213,#11214);
#9744=AXIS2_PLACEMENT_3D('',#14178,#11215,#11216);
#9745=AXIS2_PLACEMENT_3D('',#14179,#11217,#11218);
#9746=AXIS2_PLACEMENT_3D('',#14184,#11220,#11221);
#9747=AXIS2_PLACEMENT_3D('',#14187,#11223,#11224);
#9748=AXIS2_PLACEMENT_3D('',#14188,#11225,#11226);
#9749=AXIS2_PLACEMENT_3D('',#14193,#11228,#11229);
#9750=AXIS2_PLACEMENT_3D('',#14196,#11231,#11232);
#9751=AXIS2_PLACEMENT_3D('',#14197,#11233,#11234);
#9752=AXIS2_PLACEMENT_3D('',#14201,#11236,#11237);
#9753=AXIS2_PLACEMENT_3D('',#14202,#11238,#11239);
#9754=AXIS2_PLACEMENT_3D('',#14212,#11240,#11241);
#9755=AXIS2_PLACEMENT_3D('',#14234,#11243,#11244);
#9756=AXIS2_PLACEMENT_3D('',#14235,#11245,#11246);
#9757=AXIS2_PLACEMENT_3D('',#14237,#11248,#11249);
#9758=AXIS2_PLACEMENT_3D('',#14238,#11250,#11251);
#9759=AXIS2_PLACEMENT_3D('',#14240,#11253,#11254);
#9760=AXIS2_PLACEMENT_3D('',#14241,#11255,#11256);
#9761=AXIS2_PLACEMENT_3D('',#14243,#11257,#11258);
#9762=AXIS2_PLACEMENT_3D('',#14244,#11259,#11260);
#9763=AXIS2_PLACEMENT_3D('',#14245,#11261,#11262);
#9764=AXIS2_PLACEMENT_3D('',#14247,#11264,#11265);
#9765=AXIS2_PLACEMENT_3D('',#14248,#11266,#11267);
#9766=AXIS2_PLACEMENT_3D('',#14250,#11268,#11269);
#9767=AXIS2_PLACEMENT_3D('',#14251,#11270,#11271);
#9768=AXIS2_PLACEMENT_3D('',#14262,#11278,#11279);
#9769=AXIS2_PLACEMENT_3D('',#14264,#11280,#11281);
#9770=AXIS2_PLACEMENT_3D('',#14266,#11283,#11284);
#9771=AXIS2_PLACEMENT_3D('',#14268,#11285,#11286);
#9772=AXIS2_PLACEMENT_3D('',#14270,#11288,#11289);
#9773=AXIS2_PLACEMENT_3D('',#14272,#11290,#11291);
#9774=AXIS2_PLACEMENT_3D('',#14276,#11294,#11295);
#9775=AXIS2_PLACEMENT_3D('',#14277,#11296,#11297);
#9776=AXIS2_PLACEMENT_3D('',#14283,#11301,#11302);
#9777=AXIS2_PLACEMENT_3D('',#14287,#11305,#11306);
#9778=AXIS2_PLACEMENT_3D('',#14291,#11309,#11310);
#9779=AXIS2_PLACEMENT_3D('',#14293,#11312,#11313);
#9780=AXIS2_PLACEMENT_3D('',#14294,#11314,#11315);
#9781=AXIS2_PLACEMENT_3D('',#14295,#11316,#11317);
#9782=AXIS2_PLACEMENT_3D('',#14297,#11318,#11319);
#9783=AXIS2_PLACEMENT_3D('',#14300,#11321,#11322);
#9784=AXIS2_PLACEMENT_3D('',#14301,#11323,#11324);
#9785=AXIS2_PLACEMENT_3D('',#14303,#11325,#11326);
#9786=AXIS2_PLACEMENT_3D('',#14306,#11328,#11329);
#9787=AXIS2_PLACEMENT_3D('',#14307,#11330,#11331);
#9788=AXIS2_PLACEMENT_3D('',#14309,#11332,#11333);
#9789=AXIS2_PLACEMENT_3D('',#14312,#11335,#11336);
#9790=AXIS2_PLACEMENT_3D('',#14313,#11337,#11338);
#9791=AXIS2_PLACEMENT_3D('',#14315,#11339,#11340);
#9792=AXIS2_PLACEMENT_3D('',#14318,#11342,#11343);
#9793=AXIS2_PLACEMENT_3D('',#14319,#11344,#11345);
#9794=AXIS2_PLACEMENT_3D('',#14321,#11346,#11347);
#9795=AXIS2_PLACEMENT_3D('',#14324,#11349,#11350);
#9796=AXIS2_PLACEMENT_3D('',#14325,#11351,#11352);
#9797=AXIS2_PLACEMENT_3D('',#14327,#11353,#11354);
#9798=AXIS2_PLACEMENT_3D('',#14330,#11356,#11357);
#9799=AXIS2_PLACEMENT_3D('',#14331,#11358,#11359);
#9800=AXIS2_PLACEMENT_3D('',#14333,#11360,#11361);
#9801=AXIS2_PLACEMENT_3D('',#14336,#11363,#11364);
#9802=AXIS2_PLACEMENT_3D('',#14337,#11365,#11366);
#9803=AXIS2_PLACEMENT_3D('',#14346,#11371,#11372);
#9804=AXIS2_PLACEMENT_3D('',#14355,#11377,#11378);
#9805=AXIS2_PLACEMENT_3D('',#14361,#11382,#11383);
#9806=AXIS2_PLACEMENT_3D('',#14367,#11387,#11388);
#9807=AXIS2_PLACEMENT_3D('',#14373,#11392,#11393);
#9808=AXIS2_PLACEMENT_3D('',#14378,#11397,#11398);
#9809=AXIS2_PLACEMENT_3D('',#14382,#11401,#11402);
#9810=AXIS2_PLACEMENT_3D('',#14385,#11405,#11406);
#9811=AXIS2_PLACEMENT_3D('',#14386,#11407,#11408);
#9812=AXIS2_PLACEMENT_3D('',#14387,#11409,#11410);
#9813=AXIS2_PLACEMENT_3D('',#14388,#11411,#11412);
#9814=AXIS2_PLACEMENT_3D('',#14390,#11413,#11414);
#9815=AXIS2_PLACEMENT_3D('',#14393,#11416,#11417);
#9816=AXIS2_PLACEMENT_3D('',#14394,#11418,#11419);
#9817=AXIS2_PLACEMENT_3D('',#14396,#11420,#11421);
#9818=AXIS2_PLACEMENT_3D('',#14399,#11423,#11424);
#9819=AXIS2_PLACEMENT_3D('',#14400,#11425,#11426);
#9820=AXIS2_PLACEMENT_3D('',#14402,#11427,#11428);
#9821=AXIS2_PLACEMENT_3D('',#14405,#11430,#11431);
#9822=AXIS2_PLACEMENT_3D('',#14406,#11432,#11433);
#9823=AXIS2_PLACEMENT_3D('',#14408,#11434,#11435);
#9824=AXIS2_PLACEMENT_3D('',#14411,#11437,#11438);
#9825=AXIS2_PLACEMENT_3D('',#14412,#11439,#11440);
#9826=AXIS2_PLACEMENT_3D('',#14414,#11441,#11442);
#9827=AXIS2_PLACEMENT_3D('',#14417,#11444,#11445);
#9828=AXIS2_PLACEMENT_3D('',#14418,#11446,#11447);
#9829=AXIS2_PLACEMENT_3D('',#14420,#11448,#11449);
#9830=AXIS2_PLACEMENT_3D('',#14421,#11450,#11451);
#9831=AXIS2_PLACEMENT_3D('',#14424,#11453,#11454);
#9832=AXIS2_PLACEMENT_3D('',#14425,#11455,#11456);
#9833=AXIS2_PLACEMENT_3D('',#14427,#11457,#11458);
#9834=AXIS2_PLACEMENT_3D('',#14430,#11460,#11461);
#9835=AXIS2_PLACEMENT_3D('',#14431,#11462,#11463);
#9836=AXIS2_PLACEMENT_3D('',#14432,#11464,#11465);
#9837=AXIS2_PLACEMENT_3D('',#14433,#11466,#11467);
#9838=AXIS2_PLACEMENT_3D('',#14434,#11468,#11469);
#9839=AXIS2_PLACEMENT_3D('',#14436,#11470,#11471);
#9840=AXIS2_PLACEMENT_3D('',#14439,#11473,#11474);
#9841=AXIS2_PLACEMENT_3D('',#14440,#11475,#11476);
#9842=AXIS2_PLACEMENT_3D('',#14442,#11477,#11478);
#9843=AXIS2_PLACEMENT_3D('',#14445,#11480,#11481);
#9844=AXIS2_PLACEMENT_3D('',#14446,#11482,#11483);
#9845=AXIS2_PLACEMENT_3D('',#14448,#11484,#11485);
#9846=AXIS2_PLACEMENT_3D('',#14451,#11487,#11488);
#9847=AXIS2_PLACEMENT_3D('',#14452,#11489,#11490);
#9848=AXIS2_PLACEMENT_3D('',#14454,#11491,#11492);
#9849=AXIS2_PLACEMENT_3D('',#14457,#11494,#11495);
#9850=AXIS2_PLACEMENT_3D('',#14458,#11496,#11497);
#9851=AXIS2_PLACEMENT_3D('',#14460,#11498,#11499);
#9852=AXIS2_PLACEMENT_3D('',#14463,#11501,#11502);
#9853=AXIS2_PLACEMENT_3D('',#14464,#11503,#11504);
#9854=AXIS2_PLACEMENT_3D('',#14466,#11505,#11506);
#9855=AXIS2_PLACEMENT_3D('',#14467,#11507,#11508);
#9856=AXIS2_PLACEMENT_3D('',#14469,#11509,#11510);
#9857=AXIS2_PLACEMENT_3D('',#14471,#11512,#11513);
#9858=AXIS2_PLACEMENT_3D('',#14473,#11514,#11515);
#9859=AXIS2_PLACEMENT_3D('',#14476,#11517,#11518);
#9860=AXIS2_PLACEMENT_3D('',#14477,#11519,#11520);
#9861=AXIS2_PLACEMENT_3D('',#14478,#11521,#11522);
#9862=AXIS2_PLACEMENT_3D('',#14479,#11523,#11524);
#9863=AXIS2_PLACEMENT_3D('',#14480,#11525,#11526);
#9864=AXIS2_PLACEMENT_3D('',#14482,#11527,#11528);
#9865=AXIS2_PLACEMENT_3D('',#14485,#11530,#11531);
#9866=AXIS2_PLACEMENT_3D('',#14486,#11532,#11533);
#9867=AXIS2_PLACEMENT_3D('',#14488,#11534,#11535);
#9868=AXIS2_PLACEMENT_3D('',#14491,#11537,#11538);
#9869=AXIS2_PLACEMENT_3D('',#14492,#11539,#11540);
#9870=AXIS2_PLACEMENT_3D('',#14494,#11541,#11542);
#9871=AXIS2_PLACEMENT_3D('',#14497,#11544,#11545);
#9872=AXIS2_PLACEMENT_3D('',#14498,#11546,#11547);
#9873=AXIS2_PLACEMENT_3D('',#14500,#11548,#11549);
#9874=AXIS2_PLACEMENT_3D('',#14503,#11551,#11552);
#9875=AXIS2_PLACEMENT_3D('',#14504,#11553,#11554);
#9876=AXIS2_PLACEMENT_3D('',#14506,#11555,#11556);
#9877=AXIS2_PLACEMENT_3D('',#14509,#11558,#11559);
#9878=AXIS2_PLACEMENT_3D('',#14510,#11560,#11561);
#9879=AXIS2_PLACEMENT_3D('',#14512,#11562,#11563);
#9880=AXIS2_PLACEMENT_3D('',#14515,#11565,#11566);
#9881=AXIS2_PLACEMENT_3D('',#14516,#11567,#11568);
#9882=AXIS2_PLACEMENT_3D('',#14518,#11569,#11570);
#9883=AXIS2_PLACEMENT_3D('',#14521,#11572,#11573);
#9884=AXIS2_PLACEMENT_3D('',#14522,#11574,#11575);
#9885=AXIS2_PLACEMENT_3D('',#14531,#11580,#11581);
#9886=AXIS2_PLACEMENT_3D('',#14540,#11586,#11587);
#9887=AXIS2_PLACEMENT_3D('',#14546,#11591,#11592);
#9888=AXIS2_PLACEMENT_3D('',#14552,#11596,#11597);
#9889=AXIS2_PLACEMENT_3D('',#14558,#11601,#11602);
#9890=AXIS2_PLACEMENT_3D('',#14563,#11606,#11607);
#9891=AXIS2_PLACEMENT_3D('',#14567,#11610,#11611);
#9892=AXIS2_PLACEMENT_3D('',#14570,#11614,#11615);
#9893=AXIS2_PLACEMENT_3D('',#14571,#11616,#11617);
#9894=AXIS2_PLACEMENT_3D('',#14572,#11618,#11619);
#9895=AXIS2_PLACEMENT_3D('',#14573,#11620,#11621);
#9896=AXIS2_PLACEMENT_3D('',#14575,#11622,#11623);
#9897=AXIS2_PLACEMENT_3D('',#14578,#11625,#11626);
#9898=AXIS2_PLACEMENT_3D('',#14579,#11627,#11628);
#9899=AXIS2_PLACEMENT_3D('',#14581,#11629,#11630);
#9900=AXIS2_PLACEMENT_3D('',#14584,#11632,#11633);
#9901=AXIS2_PLACEMENT_3D('',#14585,#11634,#11635);
#9902=AXIS2_PLACEMENT_3D('',#14587,#11636,#11637);
#9903=AXIS2_PLACEMENT_3D('',#14590,#11639,#11640);
#9904=AXIS2_PLACEMENT_3D('',#14591,#11641,#11642);
#9905=AXIS2_PLACEMENT_3D('',#14593,#11643,#11644);
#9906=AXIS2_PLACEMENT_3D('',#14596,#11646,#11647);
#9907=AXIS2_PLACEMENT_3D('',#14597,#11648,#11649);
#9908=AXIS2_PLACEMENT_3D('',#14599,#11650,#11651);
#9909=AXIS2_PLACEMENT_3D('',#14602,#11653,#11654);
#9910=AXIS2_PLACEMENT_3D('',#14603,#11655,#11656);
#9911=AXIS2_PLACEMENT_3D('',#14605,#11657,#11658);
#9912=AXIS2_PLACEMENT_3D('',#14606,#11659,#11660);
#9913=AXIS2_PLACEMENT_3D('',#14609,#11662,#11663);
#9914=AXIS2_PLACEMENT_3D('',#14610,#11664,#11665);
#9915=AXIS2_PLACEMENT_3D('',#14612,#11666,#11667);
#9916=AXIS2_PLACEMENT_3D('',#14615,#11669,#11670);
#9917=AXIS2_PLACEMENT_3D('',#14616,#11671,#11672);
#9918=AXIS2_PLACEMENT_3D('',#14617,#11673,#11674);
#9919=AXIS2_PLACEMENT_3D('',#14618,#11675,#11676);
#9920=AXIS2_PLACEMENT_3D('',#14619,#11677,#11678);
#9921=AXIS2_PLACEMENT_3D('',#14621,#11679,#11680);
#9922=AXIS2_PLACEMENT_3D('',#14624,#11682,#11683);
#9923=AXIS2_PLACEMENT_3D('',#14625,#11684,#11685);
#9924=AXIS2_PLACEMENT_3D('',#14627,#11686,#11687);
#9925=AXIS2_PLACEMENT_3D('',#14630,#11689,#11690);
#9926=AXIS2_PLACEMENT_3D('',#14631,#11691,#11692);
#9927=AXIS2_PLACEMENT_3D('',#14633,#11693,#11694);
#9928=AXIS2_PLACEMENT_3D('',#14636,#11696,#11697);
#9929=AXIS2_PLACEMENT_3D('',#14637,#11698,#11699);
#9930=AXIS2_PLACEMENT_3D('',#14639,#11700,#11701);
#9931=AXIS2_PLACEMENT_3D('',#14642,#11703,#11704);
#9932=AXIS2_PLACEMENT_3D('',#14643,#11705,#11706);
#9933=AXIS2_PLACEMENT_3D('',#14645,#11707,#11708);
#9934=AXIS2_PLACEMENT_3D('',#14648,#11710,#11711);
#9935=AXIS2_PLACEMENT_3D('',#14649,#11712,#11713);
#9936=AXIS2_PLACEMENT_3D('',#14651,#11714,#11715);
#9937=AXIS2_PLACEMENT_3D('',#14652,#11716,#11717);
#9938=AXIS2_PLACEMENT_3D('',#14654,#11718,#11719);
#9939=AXIS2_PLACEMENT_3D('',#14656,#11721,#11722);
#9940=AXIS2_PLACEMENT_3D('',#14658,#11723,#11724);
#9941=AXIS2_PLACEMENT_3D('',#14661,#11726,#11727);
#9942=AXIS2_PLACEMENT_3D('',#14662,#11728,#11729);
#9943=AXIS2_PLACEMENT_3D('',#14663,#11730,#11731);
#9944=AXIS2_PLACEMENT_3D('',#14664,#11732,#11733);
#9945=AXIS2_PLACEMENT_3D('',#14665,#11734,#11735);
#9946=AXIS2_PLACEMENT_3D('',#14667,#11736,#11737);
#9947=AXIS2_PLACEMENT_3D('',#14670,#11739,#11740);
#9948=AXIS2_PLACEMENT_3D('',#14671,#11741,#11742);
#9949=AXIS2_PLACEMENT_3D('',#14673,#11743,#11744);
#9950=AXIS2_PLACEMENT_3D('',#14675,#11746,#11747);
#9951=AXIS2_PLACEMENT_3D('',#14676,#11748,#11749);
#9952=AXIS2_PLACEMENT_3D('',#14678,#11750,#11751);
#9953=AXIS2_PLACEMENT_3D('',#14680,#11753,#11754);
#9954=AXIS2_PLACEMENT_3D('',#14681,#11755,#11756);
#9955=AXIS2_PLACEMENT_3D('',#14682,#11757,#11758);
#9956=AXIS2_PLACEMENT_3D('',#14683,#11759,#11760);
#9957=AXIS2_PLACEMENT_3D('',#14686,#11761,#11762);
#9958=AXIS2_PLACEMENT_3D('',#14687,#11763,#11764);
#9959=AXIS2_PLACEMENT_3D('',#14689,#11765,#11766);
#9960=AXIS2_PLACEMENT_3D('',#14691,#11767,#11768);
#9961=AXIS2_PLACEMENT_3D('',#14692,#11769,#11770);
#9962=AXIS2_PLACEMENT_3D('',#14693,#11771,#11772);
#9963=AXIS2_PLACEMENT_3D('',#14696,#11774,#11775);
#9964=AXIS2_PLACEMENT_3D('',#14697,#11776,#11777);
#9965=AXIS2_PLACEMENT_3D('',#14699,#11778,#11779);
#9966=AXIS2_PLACEMENT_3D('',#14702,#11781,#11782);
#9967=AXIS2_PLACEMENT_3D('',#14703,#11783,#11784);
#9968=AXIS2_PLACEMENT_3D('',#14706,#11786,#11787);
#9969=AXIS2_PLACEMENT_3D('',#14707,#11788,#11789);
#9970=AXIS2_PLACEMENT_3D('',#14708,#11790,#11791);
#9971=AXIS2_PLACEMENT_3D('',#14710,#11792,#11793);
#9972=AXIS2_PLACEMENT_3D('',#14712,#11795,#11796);
#9973=AXIS2_PLACEMENT_3D('',#14714,#11797,#11798);
#9974=AXIS2_PLACEMENT_3D('',#14715,#11799,#11800);
#9975=AXIS2_PLACEMENT_3D('',#14717,#11802,#11803);
#9976=AXIS2_PLACEMENT_3D('',#14718,#11804,#11805);
#9977=AXIS2_PLACEMENT_3D('',#14721,#11806,#11807);
#9978=AXIS2_PLACEMENT_3D('',#14722,#11808,#11809);
#9979=AXIS2_PLACEMENT_3D('',#14724,#11810,#11811);
#9980=AXIS2_PLACEMENT_3D('',#14726,#11812,#11813);
#9981=AXIS2_PLACEMENT_3D('',#14727,#11814,#11815);
#9982=AXIS2_PLACEMENT_3D('',#14728,#11816,#11817);
#9983=AXIS2_PLACEMENT_3D('',#14730,#11818,#11819);
#9984=AXIS2_PLACEMENT_3D('',#14732,#11821,#11822);
#9985=AXIS2_PLACEMENT_3D('',#14734,#11823,#11824);
#9986=AXIS2_PLACEMENT_3D('',#14736,#11825,#11826);
#9987=AXIS2_PLACEMENT_3D('',#14737,#11827,#11828);
#9988=AXIS2_PLACEMENT_3D('',#14739,#11829,#11830);
#9989=AXIS2_PLACEMENT_3D('',#14741,#11832,#11833);
#9990=AXIS2_PLACEMENT_3D('',#14743,#11834,#11835);
#9991=AXIS2_PLACEMENT_3D('',#14745,#11837,#11838);
#9992=AXIS2_PLACEMENT_3D('',#14747,#11839,#11840);
#9993=AXIS2_PLACEMENT_3D('',#14749,#11842,#11843);
#9994=AXIS2_PLACEMENT_3D('',#14750,#11844,#11845);
#9995=AXIS2_PLACEMENT_3D('',#14752,#11847,#11848);
#9996=AXIS2_PLACEMENT_3D('',#14753,#11849,#11850);
#9997=AXIS2_PLACEMENT_3D('',#14756,#11851,#11852);
#9998=AXIS2_PLACEMENT_3D('',#14757,#11853,#11854);
#9999=AXIS2_PLACEMENT_3D('',#14760,#11855,#11856);
#10000=AXIS2_PLACEMENT_3D('',#14761,#11857,#11858);
#10001=AXIS2_PLACEMENT_3D('',#14764,#11859,#11860);
#10002=AXIS2_PLACEMENT_3D('',#14765,#11861,#11862);
#10003=AXIS2_PLACEMENT_3D('',#14768,#11863,#11864);
#10004=AXIS2_PLACEMENT_3D('',#14769,#11865,#11866);
#10005=AXIS2_PLACEMENT_3D('',#14772,#11867,#11868);
#10006=AXIS2_PLACEMENT_3D('',#14773,#11869,#11870);
#10007=AXIS2_PLACEMENT_3D('',#14776,#11871,#11872);
#10008=AXIS2_PLACEMENT_3D('',#14777,#11873,#11874);
#10009=AXIS2_PLACEMENT_3D('',#14780,#11875,#11876);
#10010=AXIS2_PLACEMENT_3D('',#14781,#11877,#11878);
#10011=AXIS2_PLACEMENT_3D('',#14782,#11879,#11880);
#10012=AXIS2_PLACEMENT_3D('',#14808,#11881,#11882);
#10013=AXIS2_PLACEMENT_3D('',#14832,#11883,#11884);
#10014=AXIS2_PLACEMENT_3D('',#14833,#11885,#11886);
#10015=AXIS2_PLACEMENT_3D('',#14835,#11887,#11888);
#10016=AXIS2_PLACEMENT_3D('',#14860,#11889,#11890);
#10017=AXIS2_PLACEMENT_3D('',#14885,#11891,#11892);
#10018=AXIS2_PLACEMENT_3D('',#14888,#11894,#11895);
#10019=AXIS2_PLACEMENT_3D('',#14890,#11896,#11897);
#10020=AXIS2_PLACEMENT_3D('',#14915,#11898,#11899);
#10021=AXIS2_PLACEMENT_3D('',#14940,#11900,#11901);
#10022=AXIS2_PLACEMENT_3D('',#14965,#11902,#11903);
#10023=AXIS2_PLACEMENT_3D('',#14989,#11904,#11905);
#10024=AXIS2_PLACEMENT_3D('',#14990,#11906,#11907);
#10025=AXIS2_PLACEMENT_3D('',#14992,#11908,#11909);
#10026=AXIS2_PLACEMENT_3D('',#14993,#11910,#11911);
#10027=AXIS2_PLACEMENT_3D('',#14994,#11912,#11913);
#10028=AXIS2_PLACEMENT_3D('',#15018,#11914,#11915);
#10029=AXIS2_PLACEMENT_3D('',#15019,#11916,#11917);
#10030=AXIS2_PLACEMENT_3D('',#15021,#11918,#11919);
#10031=AXIS2_PLACEMENT_3D('',#15022,#11920,#11921);
#10032=AXIS2_PLACEMENT_3D('',#15023,#11922,#11923);
#10033=AXIS2_PLACEMENT_3D('',#15047,#11924,#11925);
#10034=AXIS2_PLACEMENT_3D('',#15048,#11926,#11927);
#10035=AXIS2_PLACEMENT_3D('',#15050,#11928,#11929);
#10036=AXIS2_PLACEMENT_3D('',#15052,#11930,#11931);
#10037=AXIS2_PLACEMENT_3D('',#15053,#11932,#11933);
#10038=AXIS2_PLACEMENT_3D('',#15054,#11934,#11935);
#10039=AXIS2_PLACEMENT_3D('',#15078,#11936,#11937);
#10040=AXIS2_PLACEMENT_3D('',#15079,#11938,#11939);
#10041=AXIS2_PLACEMENT_3D('',#15081,#11940,#11941);
#10042=AXIS2_PLACEMENT_3D('',#15082,#11942,#11943);
#10043=AXIS2_PLACEMENT_3D('',#15083,#11944,#11945);
#10044=AXIS2_PLACEMENT_3D('',#15107,#11946,#11947);
#10045=AXIS2_PLACEMENT_3D('',#15108,#11948,#11949);
#10046=AXIS2_PLACEMENT_3D('',#15110,#11950,#11951);
#10047=AXIS2_PLACEMENT_3D('',#15111,#11952,#11953);
#10048=AXIS2_PLACEMENT_3D('',#15112,#11954,#11955);
#10049=AXIS2_PLACEMENT_3D('',#15136,#11956,#11957);
#10050=AXIS2_PLACEMENT_3D('',#15137,#11958,#11959);
#10051=AXIS2_PLACEMENT_3D('',#15139,#11960,#11961);
#10052=AXIS2_PLACEMENT_3D('',#15142,#11963,#11964);
#10053=AXIS2_PLACEMENT_3D('',#15166,#11965,#11966);
#10054=AXIS2_PLACEMENT_3D('',#15167,#11967,#11968);
#10055=AXIS2_PLACEMENT_3D('',#15168,#11969,#11970);
#10056=AXIS2_PLACEMENT_3D('',#15169,#11971,#11972);
#10057=AXIS2_PLACEMENT_3D('',#15170,#11973,#11974);
#10058=AXIS2_PLACEMENT_3D('',#15171,#11975,#11976);
#10059=AXIS2_PLACEMENT_3D('',#15172,#11977,#11978);
#10060=AXIS2_PLACEMENT_3D('',#15173,#11979,#11980);
#10061=AXIS2_PLACEMENT_3D('',#15174,#11981,#11982);
#10062=AXIS2_PLACEMENT_3D('',#15176,#11983,#11984);
#10063=AXIS2_PLACEMENT_3D('',#15178,#11985,#11986);
#10064=AXIS2_PLACEMENT_3D('',#15179,#11987,#11988);
#10065=AXIS2_PLACEMENT_3D('',#15181,#11989,#11990);
#10066=AXIS2_PLACEMENT_3D('',#15183,#11992,#11993);
#10067=AXIS2_PLACEMENT_3D('',#15185,#11994,#11995);
#10068=AXIS2_PLACEMENT_3D('',#15186,#11996,#11997);
#10069=AXIS2_PLACEMENT_3D('',#15188,#11999,#12000);
#10070=AXIS2_PLACEMENT_3D('',#15190,#12001,#12002);
#10071=AXIS2_PLACEMENT_3D('',#15192,#12003,#12004);
#10072=AXIS2_PLACEMENT_3D('',#15193,#12005,#12006);
#10073=AXIS2_PLACEMENT_3D('',#15195,#12007,#12008);
#10074=AXIS2_PLACEMENT_3D('',#15197,#12010,#12011);
#10075=AXIS2_PLACEMENT_3D('',#15199,#12012,#12013);
#10076=AXIS2_PLACEMENT_3D('',#15200,#12014,#12015);
#10077=AXIS2_PLACEMENT_3D('',#15202,#12017,#12018);
#10078=AXIS2_PLACEMENT_3D('',#15203,#12019,#12020);
#10079=AXIS2_PLACEMENT_3D('',#15204,#12021,#12022);
#10080=AXIS2_PLACEMENT_3D('',#15205,#12023,#12024);
#10081=AXIS2_PLACEMENT_3D('',#15206,#12025,#12026);
#10082=AXIS2_PLACEMENT_3D('',#15207,#12027,#12028);
#10083=AXIS2_PLACEMENT_3D('',#15208,#12029,#12030);
#10084=AXIS2_PLACEMENT_3D('',#15209,#12031,#12032);
#10085=AXIS2_PLACEMENT_3D('',#15211,#12033,#12034);
#10086=AXIS2_PLACEMENT_3D('',#15214,#12036,#12037);
#10087=AXIS2_PLACEMENT_3D('',#15215,#12038,#12039);
#10088=AXIS2_PLACEMENT_3D('',#15216,#12040,#12041);
#10089=AXIS2_PLACEMENT_3D('',#15218,#12042,#12043);
#10090=AXIS2_PLACEMENT_3D('',#15221,#12045,#12046);
#10091=AXIS2_PLACEMENT_3D('',#15222,#12047,#12048);
#10092=AXIS2_PLACEMENT_3D('',#15223,#12049,#12050);
#10093=AXIS2_PLACEMENT_3D('',#15225,#12051,#12052);
#10094=AXIS2_PLACEMENT_3D('',#15228,#12054,#12055);
#10095=AXIS2_PLACEMENT_3D('',#15229,#12056,#12057);
#10096=AXIS2_PLACEMENT_3D('',#15230,#12058,#12059);
#10097=AXIS2_PLACEMENT_3D('',#15232,#12060,#12061);
#10098=AXIS2_PLACEMENT_3D('',#15235,#12063,#12064);
#10099=AXIS2_PLACEMENT_3D('',#15236,#12065,#12066);
#10100=AXIS2_PLACEMENT_3D('',#15237,#12067,#12068);
#10101=AXIS2_PLACEMENT_3D('',#15239,#12069,#12070);
#10102=AXIS2_PLACEMENT_3D('',#15242,#12072,#12073);
#10103=AXIS2_PLACEMENT_3D('',#15243,#12074,#12075);
#10104=AXIS2_PLACEMENT_3D('',#15244,#12076,#12077);
#10105=AXIS2_PLACEMENT_3D('',#15246,#12078,#12079);
#10106=AXIS2_PLACEMENT_3D('',#15249,#12081,#12082);
#10107=AXIS2_PLACEMENT_3D('',#15250,#12083,#12084);
#10108=AXIS2_PLACEMENT_3D('',#15251,#12085,#12086);
#10109=AXIS2_PLACEMENT_3D('',#15253,#12087,#12088);
#10110=AXIS2_PLACEMENT_3D('',#15256,#12090,#12091);
#10111=AXIS2_PLACEMENT_3D('',#15257,#12092,#12093);
#10112=AXIS2_PLACEMENT_3D('',#15259,#12094,#12095);
#10113=AXIS2_PLACEMENT_3D('',#15262,#12097,#12098);
#10114=AXIS2_PLACEMENT_3D('',#15263,#12099,#12100);
#10115=AXIS2_PLACEMENT_3D('',#15265,#12101,#12102);
#10116=AXIS2_PLACEMENT_3D('',#15268,#12104,#12105);
#10117=AXIS2_PLACEMENT_3D('',#15269,#12106,#12107);
#10118=AXIS2_PLACEMENT_3D('',#15271,#12108,#12109);
#10119=AXIS2_PLACEMENT_3D('',#15274,#12111,#12112);
#10120=AXIS2_PLACEMENT_3D('',#15275,#12113,#12114);
#10121=AXIS2_PLACEMENT_3D('',#15277,#12115,#12116);
#10122=AXIS2_PLACEMENT_3D('',#15280,#12118,#12119);
#10123=AXIS2_PLACEMENT_3D('',#15281,#12120,#12121);
#10124=AXIS2_PLACEMENT_3D('',#15283,#12122,#12123);
#10125=AXIS2_PLACEMENT_3D('',#15286,#12125,#12126);
#10126=AXIS2_PLACEMENT_3D('',#15287,#12127,#12128);
#10127=AXIS2_PLACEMENT_3D('',#15289,#12129,#12130);
#10128=AXIS2_PLACEMENT_3D('',#15292,#12132,#12133);
#10129=AXIS2_PLACEMENT_3D('',#15293,#12134,#12135);
#10130=AXIS2_PLACEMENT_3D('',#15302,#12140,#12141);
#10131=AXIS2_PLACEMENT_3D('',#15308,#12145,#12146);
#10132=AXIS2_PLACEMENT_3D('',#15314,#12150,#12151);
#10133=AXIS2_PLACEMENT_3D('',#15317,#12154,#12155);
#10134=AXIS2_PLACEMENT_3D('',#15318,#12156,#12157);
#10135=AXIS2_PLACEMENT_3D('',#15319,#12158,#12159);
#10136=AXIS2_PLACEMENT_3D('',#15320,#12160,#12161);
#10137=AXIS2_PLACEMENT_3D('',#15322,#12162,#12163);
#10138=AXIS2_PLACEMENT_3D('',#15325,#12165,#12166);
#10139=AXIS2_PLACEMENT_3D('',#15326,#12167,#12168);
#10140=AXIS2_PLACEMENT_3D('',#15328,#12169,#12170);
#10141=AXIS2_PLACEMENT_3D('',#15331,#12172,#12173);
#10142=AXIS2_PLACEMENT_3D('',#15332,#12174,#12175);
#10143=AXIS2_PLACEMENT_3D('',#15334,#12176,#12177);
#10144=AXIS2_PLACEMENT_3D('',#15337,#12179,#12180);
#10145=AXIS2_PLACEMENT_3D('',#15338,#12181,#12182);
#10146=AXIS2_PLACEMENT_3D('',#15340,#12183,#12184);
#10147=AXIS2_PLACEMENT_3D('',#15343,#12186,#12187);
#10148=AXIS2_PLACEMENT_3D('',#15344,#12188,#12189);
#10149=AXIS2_PLACEMENT_3D('',#15346,#12190,#12191);
#10150=AXIS2_PLACEMENT_3D('',#15349,#12193,#12194);
#10151=AXIS2_PLACEMENT_3D('',#15350,#12195,#12196);
#10152=AXIS2_PLACEMENT_3D('',#15352,#12197,#12198);
#10153=AXIS2_PLACEMENT_3D('',#15355,#12200,#12201);
#10154=AXIS2_PLACEMENT_3D('',#15356,#12202,#12203);
#10155=AXIS2_PLACEMENT_3D('',#15358,#12204,#12205);
#10156=AXIS2_PLACEMENT_3D('',#15361,#12207,#12208);
#10157=AXIS2_PLACEMENT_3D('',#15362,#12209,#12210);
#10158=AXIS2_PLACEMENT_3D('',#15371,#12215,#12216);
#10159=AXIS2_PLACEMENT_3D('',#15377,#12220,#12221);
#10160=AXIS2_PLACEMENT_3D('',#15383,#12225,#12226);
#10161=AXIS2_PLACEMENT_3D('',#15386,#12229,#12230);
#10162=AXIS2_PLACEMENT_3D('',#15387,#12231,#12232);
#10163=AXIS2_PLACEMENT_3D('',#15388,#12233,#12234);
#10164=AXIS2_PLACEMENT_3D('',#15389,#12235,#12236);
#10165=AXIS2_PLACEMENT_3D('',#15391,#12237,#12238);
#10166=AXIS2_PLACEMENT_3D('',#15394,#12240,#12241);
#10167=AXIS2_PLACEMENT_3D('',#15395,#12242,#12243);
#10168=AXIS2_PLACEMENT_3D('',#15397,#12244,#12245);
#10169=AXIS2_PLACEMENT_3D('',#15400,#12247,#12248);
#10170=AXIS2_PLACEMENT_3D('',#15401,#12249,#12250);
#10171=AXIS2_PLACEMENT_3D('',#15403,#12251,#12252);
#10172=AXIS2_PLACEMENT_3D('',#15406,#12254,#12255);
#10173=AXIS2_PLACEMENT_3D('',#15407,#12256,#12257);
#10174=AXIS2_PLACEMENT_3D('',#15409,#12258,#12259);
#10175=AXIS2_PLACEMENT_3D('',#15412,#12261,#12262);
#10176=AXIS2_PLACEMENT_3D('',#15413,#12263,#12264);
#10177=AXIS2_PLACEMENT_3D('',#15415,#12265,#12266);
#10178=AXIS2_PLACEMENT_3D('',#15418,#12268,#12269);
#10179=AXIS2_PLACEMENT_3D('',#15419,#12270,#12271);
#10180=AXIS2_PLACEMENT_3D('',#15421,#12272,#12273);
#10181=AXIS2_PLACEMENT_3D('',#15424,#12275,#12276);
#10182=AXIS2_PLACEMENT_3D('',#15425,#12277,#12278);
#10183=AXIS2_PLACEMENT_3D('',#15427,#12279,#12280);
#10184=AXIS2_PLACEMENT_3D('',#15430,#12282,#12283);
#10185=AXIS2_PLACEMENT_3D('',#15431,#12284,#12285);
#10186=AXIS2_PLACEMENT_3D('',#15440,#12290,#12291);
#10187=AXIS2_PLACEMENT_3D('',#15446,#12295,#12296);
#10188=AXIS2_PLACEMENT_3D('',#15452,#12300,#12301);
#10189=AXIS2_PLACEMENT_3D('',#15455,#12304,#12305);
#10190=AXIS2_PLACEMENT_3D('',#15456,#12306,#12307);
#10191=AXIS2_PLACEMENT_3D('',#15457,#12308,#12309);
#10192=AXIS2_PLACEMENT_3D('',#15458,#12310,#12311);
#10193=AXIS2_PLACEMENT_3D('',#15461,#12312,#12313);
#10194=AXIS2_PLACEMENT_3D('',#15463,#12314,#12315);
#10195=AXIS2_PLACEMENT_3D('',#15464,#12316,#12317);
#10196=AXIS2_PLACEMENT_3D('',#15465,#12318,#12319);
#10197=AXIS2_PLACEMENT_3D('',#15469,#12321,#12322);
#10198=AXIS2_PLACEMENT_3D('',#15473,#12325,#12326);
#10199=AXIS2_PLACEMENT_3D('',#15474,#12327,#12328);
#10200=AXIS2_PLACEMENT_3D('',#15477,#12329,#12330);
#10201=AXIS2_PLACEMENT_3D('',#15479,#12331,#12332);
#10202=AXIS2_PLACEMENT_3D('',#15480,#12333,#12334);
#10203=AXIS2_PLACEMENT_3D('',#15481,#12335,#12336);
#10204=AXIS2_PLACEMENT_3D('',#15485,#12338,#12339);
#10205=AXIS2_PLACEMENT_3D('',#15488,#12341,#12342);
#10206=AXIS2_PLACEMENT_3D('',#15490,#12343,#12344);
#10207=AXIS2_PLACEMENT_3D('',#15492,#12346,#12347);
#10208=AXIS2_PLACEMENT_3D('',#15493,#12348,#12349);
#10209=AXIS2_PLACEMENT_3D('',#15496,#12351,#12352);
#10210=AXIS2_PLACEMENT_3D('',#15497,#12353,#12354);
#10211=AXIS2_PLACEMENT_3D('',#15498,#12355,#12356);
#10212=AXIS2_PLACEMENT_3D('',#15500,#12357,#12358);
#10213=AXIS2_PLACEMENT_3D('',#15501,#12359,#12360);
#10214=AXIS2_PLACEMENT_3D('',#15503,#12361,#12362);
#10215=AXIS2_PLACEMENT_3D('',#15505,#12364,#12365);
#10216=AXIS2_PLACEMENT_3D('',#15507,#12366,#12367);
#10217=AXIS2_PLACEMENT_3D('',#15508,#12368,#12369);
#10218=AXIS2_PLACEMENT_3D('',#15511,#12371,#12372);
#10219=AXIS2_PLACEMENT_3D('',#15512,#12373,#12374);
#10220=AXIS2_PLACEMENT_3D('',#15513,#12375,#12376);
#10221=AXIS2_PLACEMENT_3D('',#15514,#12377,#12378);
#10222=AXIS2_PLACEMENT_3D('',#15516,#12379,#12380);
#10223=AXIS2_PLACEMENT_3D('',#15519,#12382,#12383);
#10224=AXIS2_PLACEMENT_3D('',#15520,#12384,#12385);
#10225=AXIS2_PLACEMENT_3D('',#15522,#12386,#12387);
#10226=AXIS2_PLACEMENT_3D('',#15523,#12388,#12389);
#10227=AXIS2_PLACEMENT_3D('',#15525,#12390,#12391);
#10228=AXIS2_PLACEMENT_3D('',#15528,#12393,#12394);
#10229=AXIS2_PLACEMENT_3D('',#15529,#12395,#12396);
#10230=AXIS2_PLACEMENT_3D('',#15531,#12397,#12398);
#10231=AXIS2_PLACEMENT_3D('',#15532,#12399,#12400);
#10232=AXIS2_PLACEMENT_3D('',#15534,#12401,#12402);
#10233=AXIS2_PLACEMENT_3D('',#15537,#12404,#12405);
#10234=AXIS2_PLACEMENT_3D('',#15538,#12406,#12407);
#10235=AXIS2_PLACEMENT_3D('',#15540,#12408,#12409);
#10236=AXIS2_PLACEMENT_3D('',#15541,#12410,#12411);
#10237=AXIS2_PLACEMENT_3D('',#15543,#12412,#12413);
#10238=AXIS2_PLACEMENT_3D('',#15546,#12415,#12416);
#10239=AXIS2_PLACEMENT_3D('',#15547,#12417,#12418);
#10240=AXIS2_PLACEMENT_3D('',#15549,#12419,#12420);
#10241=AXIS2_PLACEMENT_3D('',#15550,#12421,#12422);
#10242=AXIS2_PLACEMENT_3D('',#15552,#12423,#12424);
#10243=AXIS2_PLACEMENT_3D('',#15554,#12426,#12427);
#10244=AXIS2_PLACEMENT_3D('',#15556,#12428,#12429);
#10245=AXIS2_PLACEMENT_3D('',#15558,#12431,#12432);
#10246=AXIS2_PLACEMENT_3D('',#15560,#12433,#12434);
#10247=AXIS2_PLACEMENT_3D('',#15562,#12436,#12437);
#10248=AXIS2_PLACEMENT_3D('',#15564,#12438,#12439);
#10249=AXIS2_PLACEMENT_3D('',#15566,#12441,#12442);
#10250=AXIS2_PLACEMENT_3D('',#15575,#12447,#12448);
#10251=AXIS2_PLACEMENT_3D('',#15581,#12452,#12453);
#10252=AXIS2_PLACEMENT_3D('',#15587,#12457,#12458);
#10253=AXIS2_PLACEMENT_3D('',#15590,#12461,#12462);
#10254=AXIS2_PLACEMENT_3D('',#15591,#12463,#12464);
#10255=AXIS2_PLACEMENT_3D('',#15592,#12465,#12466);
#10256=AXIS2_PLACEMENT_3D('',#15593,#12467,#12468);
#10257=AXIS2_PLACEMENT_3D('',#15594,#12469,#12470);
#10258=AXIS2_PLACEMENT_3D('',#15596,#12471,#12472);
#10259=AXIS2_PLACEMENT_3D('',#15599,#12474,#12475);
#10260=AXIS2_PLACEMENT_3D('',#15600,#12476,#12477);
#10261=AXIS2_PLACEMENT_3D('',#15601,#12478,#12479);
#10262=AXIS2_PLACEMENT_3D('',#15603,#12480,#12481);
#10263=AXIS2_PLACEMENT_3D('',#15606,#12483,#12484);
#10264=AXIS2_PLACEMENT_3D('',#15607,#12485,#12486);
#10265=AXIS2_PLACEMENT_3D('',#15608,#12487,#12488);
#10266=AXIS2_PLACEMENT_3D('',#15610,#12489,#12490);
#10267=AXIS2_PLACEMENT_3D('',#15613,#12492,#12493);
#10268=AXIS2_PLACEMENT_3D('',#15614,#12494,#12495);
#10269=AXIS2_PLACEMENT_3D('',#15615,#12496,#12497);
#10270=AXIS2_PLACEMENT_3D('',#15617,#12498,#12499);
#10271=AXIS2_PLACEMENT_3D('',#15620,#12501,#12502);
#10272=AXIS2_PLACEMENT_3D('',#15621,#12503,#12504);
#10273=AXIS2_PLACEMENT_3D('',#15622,#12505,#12506);
#10274=AXIS2_PLACEMENT_3D('',#15624,#12507,#12508);
#10275=AXIS2_PLACEMENT_3D('',#15627,#12510,#12511);
#10276=AXIS2_PLACEMENT_3D('',#15628,#12512,#12513);
#10277=AXIS2_PLACEMENT_3D('',#15629,#12514,#12515);
#10278=AXIS2_PLACEMENT_3D('',#15631,#12516,#12517);
#10279=AXIS2_PLACEMENT_3D('',#15634,#12519,#12520);
#10280=AXIS2_PLACEMENT_3D('',#15635,#12521,#12522);
#10281=AXIS2_PLACEMENT_3D('',#15636,#12523,#12524);
#10282=AXIS2_PLACEMENT_3D('',#15638,#12525,#12526);
#10283=AXIS2_PLACEMENT_3D('',#15641,#12528,#12529);
#10284=AXIS2_PLACEMENT_3D('',#15642,#12530,#12531);
#10285=AXIS2_PLACEMENT_3D('',#15644,#12532,#12533);
#10286=AXIS2_PLACEMENT_3D('',#15647,#12535,#12536);
#10287=AXIS2_PLACEMENT_3D('',#15648,#12537,#12538);
#10288=AXIS2_PLACEMENT_3D('',#15650,#12539,#12540);
#10289=AXIS2_PLACEMENT_3D('',#15653,#12542,#12543);
#10290=AXIS2_PLACEMENT_3D('',#15654,#12544,#12545);
#10291=AXIS2_PLACEMENT_3D('',#15656,#12546,#12547);
#10292=AXIS2_PLACEMENT_3D('',#15659,#12549,#12550);
#10293=AXIS2_PLACEMENT_3D('',#15660,#12551,#12552);
#10294=AXIS2_PLACEMENT_3D('',#15662,#12553,#12554);
#10295=AXIS2_PLACEMENT_3D('',#15665,#12556,#12557);
#10296=AXIS2_PLACEMENT_3D('',#15666,#12558,#12559);
#10297=AXIS2_PLACEMENT_3D('',#15668,#12560,#12561);
#10298=AXIS2_PLACEMENT_3D('',#15671,#12563,#12564);
#10299=AXIS2_PLACEMENT_3D('',#15672,#12565,#12566);
#10300=AXIS2_PLACEMENT_3D('',#15674,#12567,#12568);
#10301=AXIS2_PLACEMENT_3D('',#15677,#12570,#12571);
#10302=AXIS2_PLACEMENT_3D('',#15678,#12572,#12573);
#10303=AXIS2_PLACEMENT_3D('',#15687,#12578,#12579);
#10304=AXIS2_PLACEMENT_3D('',#15693,#12583,#12584);
#10305=AXIS2_PLACEMENT_3D('',#15699,#12588,#12589);
#10306=AXIS2_PLACEMENT_3D('',#15702,#12592,#12593);
#10307=AXIS2_PLACEMENT_3D('',#15703,#12594,#12595);
#10308=AXIS2_PLACEMENT_3D('',#15704,#12596,#12597);
#10309=AXIS2_PLACEMENT_3D('',#15705,#12598,#12599);
#10310=AXIS2_PLACEMENT_3D('',#15707,#12600,#12601);
#10311=AXIS2_PLACEMENT_3D('',#15710,#12603,#12604);
#10312=AXIS2_PLACEMENT_3D('',#15711,#12605,#12606);
#10313=AXIS2_PLACEMENT_3D('',#15713,#12607,#12608);
#10314=AXIS2_PLACEMENT_3D('',#15716,#12610,#12611);
#10315=AXIS2_PLACEMENT_3D('',#15717,#12612,#12613);
#10316=AXIS2_PLACEMENT_3D('',#15719,#12614,#12615);
#10317=AXIS2_PLACEMENT_3D('',#15722,#12617,#12618);
#10318=AXIS2_PLACEMENT_3D('',#15723,#12619,#12620);
#10319=AXIS2_PLACEMENT_3D('',#15725,#12621,#12622);
#10320=AXIS2_PLACEMENT_3D('',#15728,#12624,#12625);
#10321=AXIS2_PLACEMENT_3D('',#15729,#12626,#12627);
#10322=AXIS2_PLACEMENT_3D('',#15731,#12628,#12629);
#10323=AXIS2_PLACEMENT_3D('',#15734,#12631,#12632);
#10324=AXIS2_PLACEMENT_3D('',#15735,#12633,#12634);
#10325=AXIS2_PLACEMENT_3D('',#15737,#12635,#12636);
#10326=AXIS2_PLACEMENT_3D('',#15740,#12638,#12639);
#10327=AXIS2_PLACEMENT_3D('',#15741,#12640,#12641);
#10328=AXIS2_PLACEMENT_3D('',#15743,#12642,#12643);
#10329=AXIS2_PLACEMENT_3D('',#15746,#12645,#12646);
#10330=AXIS2_PLACEMENT_3D('',#15747,#12647,#12648);
#10331=AXIS2_PLACEMENT_3D('',#15756,#12653,#12654);
#10332=AXIS2_PLACEMENT_3D('',#15762,#12658,#12659);
#10333=AXIS2_PLACEMENT_3D('',#15768,#12663,#12664);
#10334=AXIS2_PLACEMENT_3D('',#15771,#12667,#12668);
#10335=AXIS2_PLACEMENT_3D('',#15772,#12669,#12670);
#10336=AXIS2_PLACEMENT_3D('',#15773,#12671,#12672);
#10337=AXIS2_PLACEMENT_3D('',#15774,#12673,#12674);
#10338=AXIS2_PLACEMENT_3D('',#15776,#12675,#12676);
#10339=AXIS2_PLACEMENT_3D('',#15779,#12678,#12679);
#10340=AXIS2_PLACEMENT_3D('',#15780,#12680,#12681);
#10341=AXIS2_PLACEMENT_3D('',#15782,#12682,#12683);
#10342=AXIS2_PLACEMENT_3D('',#15785,#12685,#12686);
#10343=AXIS2_PLACEMENT_3D('',#15786,#12687,#12688);
#10344=AXIS2_PLACEMENT_3D('',#15788,#12689,#12690);
#10345=AXIS2_PLACEMENT_3D('',#15791,#12692,#12693);
#10346=AXIS2_PLACEMENT_3D('',#15792,#12694,#12695);
#10347=AXIS2_PLACEMENT_3D('',#15794,#12696,#12697);
#10348=AXIS2_PLACEMENT_3D('',#15797,#12699,#12700);
#10349=AXIS2_PLACEMENT_3D('',#15798,#12701,#12702);
#10350=AXIS2_PLACEMENT_3D('',#15800,#12703,#12704);
#10351=AXIS2_PLACEMENT_3D('',#15803,#12706,#12707);
#10352=AXIS2_PLACEMENT_3D('',#15804,#12708,#12709);
#10353=AXIS2_PLACEMENT_3D('',#15806,#12710,#12711);
#10354=AXIS2_PLACEMENT_3D('',#15809,#12713,#12714);
#10355=AXIS2_PLACEMENT_3D('',#15810,#12715,#12716);
#10356=AXIS2_PLACEMENT_3D('',#15812,#12717,#12718);
#10357=AXIS2_PLACEMENT_3D('',#15815,#12720,#12721);
#10358=AXIS2_PLACEMENT_3D('',#15816,#12722,#12723);
#10359=AXIS2_PLACEMENT_3D('',#15825,#12728,#12729);
#10360=AXIS2_PLACEMENT_3D('',#15831,#12733,#12734);
#10361=AXIS2_PLACEMENT_3D('',#15837,#12738,#12739);
#10362=AXIS2_PLACEMENT_3D('',#15840,#12742,#12743);
#10363=AXIS2_PLACEMENT_3D('',#15841,#12744,#12745);
#10364=AXIS2_PLACEMENT_3D('',#15842,#12746,#12747);
#10365=AXIS2_PLACEMENT_3D('',#15843,#12748,#12749);
#10366=AXIS2_PLACEMENT_3D('',#15846,#12750,#12751);
#10367=AXIS2_PLACEMENT_3D('',#15848,#12752,#12753);
#10368=AXIS2_PLACEMENT_3D('',#15849,#12754,#12755);
#10369=AXIS2_PLACEMENT_3D('',#15850,#12756,#12757);
#10370=AXIS2_PLACEMENT_3D('',#15852,#12758,#12759);
#10371=AXIS2_PLACEMENT_3D('',#15857,#12762,#12763);
#10372=AXIS2_PLACEMENT_3D('',#15859,#12765,#12766);
#10373=AXIS2_PLACEMENT_3D('',#15862,#12767,#12768);
#10374=AXIS2_PLACEMENT_3D('',#15864,#12769,#12770);
#10375=AXIS2_PLACEMENT_3D('',#15865,#12771,#12772);
#10376=AXIS2_PLACEMENT_3D('',#15866,#12773,#12774);
#10377=AXIS2_PLACEMENT_3D('',#15868,#12775,#12776);
#10378=AXIS2_PLACEMENT_3D('',#15872,#12778,#12779);
#10379=AXIS2_PLACEMENT_3D('',#15876,#12782,#12783);
#10380=AXIS2_PLACEMENT_3D('',#15877,#12784,#12785);
#10381=AXIS2_PLACEMENT_3D('',#15879,#12786,#12787);
#10382=AXIS2_PLACEMENT_3D('',#15881,#12789,#12790);
#10383=AXIS2_PLACEMENT_3D('',#15882,#12791,#12792);
#10384=AXIS2_PLACEMENT_3D('',#15883,#12793,#12794);
#10385=AXIS2_PLACEMENT_3D('',#15885,#12795,#12796);
#10386=AXIS2_PLACEMENT_3D('',#15886,#12797,#12798);
#10387=AXIS2_PLACEMENT_3D('',#15889,#12800,#12801);
#10388=AXIS2_PLACEMENT_3D('',#15890,#12802,#12803);
#10389=AXIS2_PLACEMENT_3D('',#15892,#12804,#12805);
#10390=AXIS2_PLACEMENT_3D('',#15893,#12806,#12807);
#10391=AXIS2_PLACEMENT_3D('',#15895,#12808,#12809);
#10392=AXIS2_PLACEMENT_3D('',#15897,#12811,#12812);
#10393=AXIS2_PLACEMENT_3D('',#15898,#12813,#12814);
#10394=AXIS2_PLACEMENT_3D('',#15899,#12815,#12816);
#10395=AXIS2_PLACEMENT_3D('',#15901,#12817,#12818);
#10396=AXIS2_PLACEMENT_3D('',#15904,#12820,#12821);
#10397=AXIS2_PLACEMENT_3D('',#15905,#12822,#12823);
#10398=AXIS2_PLACEMENT_3D('',#15907,#12824,#12825);
#10399=AXIS2_PLACEMENT_3D('',#15908,#12826,#12827);
#10400=AXIS2_PLACEMENT_3D('',#15910,#12828,#12829);
#10401=AXIS2_PLACEMENT_3D('',#15913,#12831,#12832);
#10402=AXIS2_PLACEMENT_3D('',#15914,#12833,#12834);
#10403=AXIS2_PLACEMENT_3D('',#15916,#12835,#12836);
#10404=AXIS2_PLACEMENT_3D('',#15917,#12837,#12838);
#10405=AXIS2_PLACEMENT_3D('',#15919,#12839,#12840);
#10406=AXIS2_PLACEMENT_3D('',#15922,#12842,#12843);
#10407=AXIS2_PLACEMENT_3D('',#15923,#12844,#12845);
#10408=AXIS2_PLACEMENT_3D('',#15925,#12846,#12847);
#10409=AXIS2_PLACEMENT_3D('',#15926,#12848,#12849);
#10410=AXIS2_PLACEMENT_3D('',#15928,#12850,#12851);
#10411=AXIS2_PLACEMENT_3D('',#15931,#12853,#12854);
#10412=AXIS2_PLACEMENT_3D('',#15932,#12855,#12856);
#10413=AXIS2_PLACEMENT_3D('',#15934,#12857,#12858);
#10414=AXIS2_PLACEMENT_3D('',#15935,#12859,#12860);
#10415=AXIS2_PLACEMENT_3D('',#15938,#12862,#12863);
#10416=AXIS2_PLACEMENT_3D('',#15939,#12864,#12865);
#10417=AXIS2_PLACEMENT_3D('',#15942,#12867,#12868);
#10418=AXIS2_PLACEMENT_3D('',#15943,#12869,#12870);
#10419=AXIS2_PLACEMENT_3D('',#15946,#12872,#12873);
#10420=AXIS2_PLACEMENT_3D('',#15947,#12874,#12875);
#10421=AXIS2_PLACEMENT_3D('',#15950,#12877,#12878);
#10422=AXIS2_PLACEMENT_3D('',#15951,#12879,#12880);
#10423=AXIS2_PLACEMENT_3D('',#15960,#12885,#12886);
#10424=AXIS2_PLACEMENT_3D('',#15966,#12890,#12891);
#10425=AXIS2_PLACEMENT_3D('',#15972,#12895,#12896);
#10426=AXIS2_PLACEMENT_3D('',#15975,#12899,#12900);
#10427=AXIS2_PLACEMENT_3D('',#15976,#12901,#12902);
#10428=AXIS2_PLACEMENT_3D('',#15977,#12903,#12904);
#10429=AXIS2_PLACEMENT_3D('',#15978,#12905,#12906);
#10430=AXIS2_PLACEMENT_3D('',#15979,#12907,#12908);
#10431=AXIS2_PLACEMENT_3D('',#15982,#12909,#12910);
#10432=AXIS2_PLACEMENT_3D('',#15988,#12914,#12915);
#10433=AXIS2_PLACEMENT_3D('',#15994,#12919,#12920);
#10434=AXIS2_PLACEMENT_3D('',#15996,#12921,#12922);
#10435=AXIS2_PLACEMENT_3D('',#16000,#12925,#12926);
#10436=AXIS2_PLACEMENT_3D('',#16003,#12929,#12930);
#10437=AXIS2_PLACEMENT_3D('',#16004,#12931,#12932);
#10438=AXIS2_PLACEMENT_3D('',#16006,#12933,#12934);
#10439=AXIS2_PLACEMENT_3D('',#16008,#12935,#12936);
#10440=AXIS2_PLACEMENT_3D('',#16009,#12937,#12938);
#10441=AXIS2_PLACEMENT_3D('',#16011,#12939,#12940);
#10442=AXIS2_PLACEMENT_3D('',#16013,#12942,#12943);
#10443=AXIS2_PLACEMENT_3D('',#16015,#12944,#12945);
#10444=AXIS2_PLACEMENT_3D('',#16016,#12946,#12947);
#10445=AXIS2_PLACEMENT_3D('',#16018,#12948,#12949);
#10446=AXIS2_PLACEMENT_3D('',#16020,#12951,#12952);
#10447=AXIS2_PLACEMENT_3D('',#16022,#12953,#12954);
#10448=AXIS2_PLACEMENT_3D('',#16023,#12955,#12956);
#10449=AXIS2_PLACEMENT_3D('',#16025,#12957,#12958);
#10450=AXIS2_PLACEMENT_3D('',#16027,#12960,#12961);
#10451=AXIS2_PLACEMENT_3D('',#16029,#12962,#12963);
#10452=AXIS2_PLACEMENT_3D('',#16030,#12964,#12965);
#10453=AXIS2_PLACEMENT_3D('',#16032,#12966,#12967);
#10454=AXIS2_PLACEMENT_3D('',#16034,#12969,#12970);
#10455=AXIS2_PLACEMENT_3D('',#16036,#12971,#12972);
#10456=AXIS2_PLACEMENT_3D('',#16037,#12973,#12974);
#10457=AXIS2_PLACEMENT_3D('',#16039,#12975,#12976);
#10458=AXIS2_PLACEMENT_3D('',#16041,#12978,#12979);
#10459=AXIS2_PLACEMENT_3D('',#16043,#12980,#12981);
#10460=AXIS2_PLACEMENT_3D('',#16044,#12982,#12983);
#10461=AXIS2_PLACEMENT_3D('',#16046,#12985,#12986);
#10462=AXIS2_PLACEMENT_3D('',#16047,#12987,#12988);
#10463=AXIS2_PLACEMENT_3D('',#16050,#12989,#12990);
#10464=AXIS2_PLACEMENT_3D('',#16054,#12992,#12993);
#10465=AXIS2_PLACEMENT_3D('',#16056,#12995,#12996);
#10466=AXIS2_PLACEMENT_3D('',#16062,#13000,#13001);
#10467=AXIS2_PLACEMENT_3D('',#16064,#13002,#13003);
#10468=AXIS2_PLACEMENT_3D('',#16066,#13004,#13005);
#10469=AXIS2_PLACEMENT_3D('',#16068,#13007,#13008);
#10470=AXIS2_PLACEMENT_3D('',#16071,#13011,#13012);
#10471=AXIS2_PLACEMENT_3D('',#16073,#13013,#13014);
#10472=AXIS2_PLACEMENT_3D('',#16075,#13015,#13016);
#10473=AXIS2_PLACEMENT_3D('',#16076,#13017,#13018);
#10474=AXIS2_PLACEMENT_3D('',#16078,#13019,#13020);
#10475=AXIS2_PLACEMENT_3D('',#16080,#13022,#13023);
#10476=AXIS2_PLACEMENT_3D('',#16082,#13024,#13025);
#10477=AXIS2_PLACEMENT_3D('',#16083,#13026,#13027);
#10478=AXIS2_PLACEMENT_3D('',#16085,#13029,#13030);
#10479=AXIS2_PLACEMENT_3D('',#16086,#13031,#13032);
#10480=AXIS2_PLACEMENT_3D('',#16087,#13033,#13034);
#10481=AXIS2_PLACEMENT_3D('',#16088,#13035,#13036);
#10482=AXIS2_PLACEMENT_3D('',#16097,#13041,#13042);
#10483=AXIS2_PLACEMENT_3D('',#16103,#13046,#13047);
#10484=AXIS2_PLACEMENT_3D('',#16109,#13051,#13052);
#10485=AXIS2_PLACEMENT_3D('',#16115,#13056,#13057);
#10486=AXIS2_PLACEMENT_3D('',#16121,#13061,#13062);
#10487=AXIS2_PLACEMENT_3D('',#16124,#13065,#13066);
#10488=AXIS2_PLACEMENT_3D('',#16125,#13067,#13068);
#10489=AXIS2_PLACEMENT_3D('',#16126,#13069,#13070);
#10490=AXIS2_PLACEMENT_3D('',#16128,#13071,#13072);
#10491=AXIS2_PLACEMENT_3D('',#16129,#13073,#13074);
#10492=AXIS2_PLACEMENT_3D('',#16131,#13075,#13076);
#10493=AXIS2_PLACEMENT_3D('',#16132,#13077,#13078);
#10494=AXIS2_PLACEMENT_3D('',#16134,#13079,#13080);
#10495=AXIS2_PLACEMENT_3D('',#16136,#13082,#13083);
#10496=AXIS2_PLACEMENT_3D('',#16138,#13084,#13085);
#10497=AXIS2_PLACEMENT_3D('',#16140,#13087,#13088);
#10498=AXIS2_PLACEMENT_3D('',#16142,#13089,#13090);
#10499=AXIS2_PLACEMENT_3D('',#16144,#13092,#13093);
#10500=AXIS2_PLACEMENT_3D('',#16146,#13094,#13095);
#10501=AXIS2_PLACEMENT_3D('',#16147,#13096,#13097);
#10502=AXIS2_PLACEMENT_3D('',#16149,#13098,#13099);
#10503=AXIS2_PLACEMENT_3D('',#16151,#13101,#13102);
#10504=AXIS2_PLACEMENT_3D('',#16153,#13104,#13105);
#10505=AXIS2_PLACEMENT_3D('',#16154,#13106,#13107);
#10506=AXIS2_PLACEMENT_3D('',#16155,#13108,#13109);
#10507=AXIS2_PLACEMENT_3D('',#16157,#13110,#13111);
#10508=AXIS2_PLACEMENT_3D('',#16160,#13113,#13114);
#10509=AXIS2_PLACEMENT_3D('',#16161,#13115,#13116);
#10510=AXIS2_PLACEMENT_3D('',#16162,#13117,#13118);
#10511=AXIS2_PLACEMENT_3D('',#16164,#13119,#13120);
#10512=AXIS2_PLACEMENT_3D('',#16167,#13122,#13123);
#10513=AXIS2_PLACEMENT_3D('',#16168,#13124,#13125);
#10514=AXIS2_PLACEMENT_3D('',#16169,#13126,#13127);
#10515=AXIS2_PLACEMENT_3D('',#16171,#13128,#13129);
#10516=AXIS2_PLACEMENT_3D('',#16173,#13130,#13131);
#10517=AXIS2_PLACEMENT_3D('',#16174,#13132,#13133);
#10518=AXIS2_PLACEMENT_3D('',#16176,#13134,#13135);
#10519=AXIS2_PLACEMENT_3D('',#16178,#13136,#13137);
#10520=AXIS2_PLACEMENT_3D('',#16179,#13138,#13139);
#10521=AXIS2_PLACEMENT_3D('',#16181,#13141,#13142);
#10522=AXIS2_PLACEMENT_3D('',#16184,#13144,#13145);
#10523=AXIS2_PLACEMENT_3D('',#16185,#13146,#13147);
#10524=AXIS2_PLACEMENT_3D('',#16187,#13148,#13149);
#10525=AXIS2_PLACEMENT_3D('',#16188,#13150,#13151);
#10526=AXIS2_PLACEMENT_3D('',#16190,#13152,#13153);
#10527=AXIS2_PLACEMENT_3D('',#16192,#13154,#13155);
#10528=AXIS2_PLACEMENT_3D('',#16193,#13156,#13157);
#10529=AXIS2_PLACEMENT_3D('',#16195,#13159,#13160);
#10530=AXIS2_PLACEMENT_3D('',#16198,#13162,#13163);
#10531=AXIS2_PLACEMENT_3D('',#16199,#13164,#13165);
#10532=AXIS2_PLACEMENT_3D('',#16201,#13166,#13167);
#10533=AXIS2_PLACEMENT_3D('',#16203,#13169,#13170);
#10534=AXIS2_PLACEMENT_3D('',#16204,#13171,#13172);
#10535=AXIS2_PLACEMENT_3D('',#16205,#13173,#13174);
#10536=AXIS2_PLACEMENT_3D('',#16206,#13175,#13176);
#10537=AXIS2_PLACEMENT_3D('',#16208,#13177,#13178);
#10538=AXIS2_PLACEMENT_3D('',#16211,#13180,#13181);
#10539=AXIS2_PLACEMENT_3D('',#16212,#13182,#13183);
#10540=AXIS2_PLACEMENT_3D('',#16214,#13184,#13185);
#10541=AXIS2_PLACEMENT_3D('',#16217,#13187,#13188);
#10542=AXIS2_PLACEMENT_3D('',#16218,#13189,#13190);
#10543=AXIS2_PLACEMENT_3D('',#16219,#13191,#13192);
#10544=AXIS2_PLACEMENT_3D('',#16220,#13193,#13194);
#10545=AXIS2_PLACEMENT_3D('',#16221,#13195,#13196);
#10546=AXIS2_PLACEMENT_3D('',#16223,#13197,#13198);
#10547=AXIS2_PLACEMENT_3D('',#16226,#13200,#13201);
#10548=AXIS2_PLACEMENT_3D('',#16227,#13202,#13203);
#10549=AXIS2_PLACEMENT_3D('',#16229,#13204,#13205);
#10550=AXIS2_PLACEMENT_3D('',#16232,#13207,#13208);
#10551=AXIS2_PLACEMENT_3D('',#16233,#13209,#13210);
#10552=AXIS2_PLACEMENT_3D('',#16234,#13211,#13212);
#10553=AXIS2_PLACEMENT_3D('',#16235,#13213,#13214);
#10554=AXIS2_PLACEMENT_3D('',#16236,#13215,#13216);
#10555=AXIS2_PLACEMENT_3D('',#16238,#13217,#13218);
#10556=AXIS2_PLACEMENT_3D('',#16241,#13220,#13221);
#10557=AXIS2_PLACEMENT_3D('',#16242,#13222,#13223);
#10558=AXIS2_PLACEMENT_3D('',#16246,#13225,#13226);
#10559=AXIS2_PLACEMENT_3D('',#16247,#13227,#13228);
#10560=AXIS2_PLACEMENT_3D('',#16257,#13229,#13230);
#10561=AXIS2_PLACEMENT_3D('',#16319,#13232,#13233);
#10562=AXIS2_PLACEMENT_3D('',#16321,#13235,#13236);
#10563=AXIS2_PLACEMENT_3D('',#16323,#13237,#13238);
#10564=AXIS2_PLACEMENT_3D('',#16324,#13239,#13240);
#10565=AXIS2_PLACEMENT_3D('',#16326,#13241,#13242);
#10566=AXIS2_PLACEMENT_3D('',#16330,#13245,#13246);
#10567=AXIS2_PLACEMENT_3D('',#16331,#13247,#13248);
#10568=AXIS2_PLACEMENT_3D('',#16333,#13249,#13250);
#10569=AXIS2_PLACEMENT_3D('',#16336,#13253,#13254);
#10570=AXIS2_PLACEMENT_3D('',#16337,#13255,#13256);
#10571=AXIS2_PLACEMENT_3D('',#16338,#13257,#13258);
#10572=AXIS2_PLACEMENT_3D('',#16339,#13259,#13260);
#10573=AXIS2_PLACEMENT_3D('',#16341,#13261,#13262);
#10574=AXIS2_PLACEMENT_3D('',#16344,#13264,#13265);
#10575=AXIS2_PLACEMENT_3D('',#16345,#13266,#13267);
#10576=AXIS2_PLACEMENT_3D('',#16347,#13268,#13269);
#10577=AXIS2_PLACEMENT_3D('',#16350,#13271,#13272);
#10578=AXIS2_PLACEMENT_3D('',#16351,#13273,#13274);
#10579=AXIS2_PLACEMENT_3D('',#16352,#13275,#13276);
#10580=AXIS2_PLACEMENT_3D('',#16353,#13277,#13278);
#10581=AXIS2_PLACEMENT_3D('',#16354,#13279,#13280);
#10582=AXIS2_PLACEMENT_3D('',#16356,#13281,#13282);
#10583=AXIS2_PLACEMENT_3D('',#16359,#13284,#13285);
#10584=AXIS2_PLACEMENT_3D('',#16360,#13286,#13287);
#10585=AXIS2_PLACEMENT_3D('',#16362,#13288,#13289);
#10586=AXIS2_PLACEMENT_3D('',#16365,#13291,#13292);
#10587=AXIS2_PLACEMENT_3D('',#16366,#13293,#13294);
#10588=AXIS2_PLACEMENT_3D('',#16367,#13295,#13296);
#10589=AXIS2_PLACEMENT_3D('',#16368,#13297,#13298);
#10590=AXIS2_PLACEMENT_3D('',#16369,#13299,#13300);
#10591=AXIS2_PLACEMENT_3D('',#16373,#13302,#13303);
#10592=AXIS2_PLACEMENT_3D('',#16374,#13304,#13305);
#10593=AXIS2_PLACEMENT_3D('',#16386,#13306,#13307);
#10594=AXIS2_PLACEMENT_3D('',#16454,#13309,#13310);
#10595=AXIS2_PLACEMENT_3D('',#16456,#13312,#13313);
#10596=AXIS2_PLACEMENT_3D('',#16458,#13314,#13315);
#10597=AXIS2_PLACEMENT_3D('',#16462,#13318,#13319);
#10598=AXIS2_PLACEMENT_3D('',#16463,#13320,#13321);
#10599=AXIS2_PLACEMENT_3D('',#16465,#13322,#13323);
#10600=AXIS2_PLACEMENT_3D('',#16469,#13326,#13327);
#10601=AXIS2_PLACEMENT_3D('',#16470,#13328,#13329);
#10602=AXIS2_PLACEMENT_3D('',#16471,#13330,#13331);
#10603=AXIS2_PLACEMENT_3D('',#16472,#13332,#13333);
#10604=AXIS2_PLACEMENT_3D('',#16473,#13334,#13335);
#10605=AXIS2_PLACEMENT_3D('',#16475,#13336,#13337);
#10606=AXIS2_PLACEMENT_3D('',#16476,#13338,#13339);
#10607=AXIS2_PLACEMENT_3D('',#16478,#13340,#13341);
#10608=AXIS2_PLACEMENT_3D('',#16480,#13343,#13344);
#10609=AXIS2_PLACEMENT_3D('',#16482,#13345,#13346);
#10610=AXIS2_PLACEMENT_3D('',#16484,#13348,#13349);
#10611=AXIS2_PLACEMENT_3D('',#16486,#13350,#13351);
#10612=AXIS2_PLACEMENT_3D('',#16488,#13353,#13354);
#10613=AXIS2_PLACEMENT_3D('',#16490,#13355,#13356);
#10614=AXIS2_PLACEMENT_3D('',#16491,#13357,#13358);
#10615=AXIS2_PLACEMENT_3D('',#16493,#13359,#13360);
#10616=AXIS2_PLACEMENT_3D('',#16495,#13362,#13363);
#10617=AXIS2_PLACEMENT_3D('',#16497,#13364,#13365);
#10618=AXIS2_PLACEMENT_3D('',#16499,#13367,#13368);
#10619=AXIS2_PLACEMENT_3D('',#16501,#13369,#13370);
#10620=AXIS2_PLACEMENT_3D('',#16503,#13372,#13373);
#10621=AXIS2_PLACEMENT_3D('',#16504,#13374,#13375);
#10622=AXIS2_PLACEMENT_3D('',#16513,#13380,#13381);
#10623=AXIS2_PLACEMENT_3D('',#16519,#13385,#13386);
#10624=AXIS2_PLACEMENT_3D('',#16525,#13390,#13391);
#10625=AXIS2_PLACEMENT_3D('',#16531,#13395,#13396);
#10626=AXIS2_PLACEMENT_3D('',#16537,#13400,#13401);
#10627=AXIS2_PLACEMENT_3D('',#16540,#13404,#13405);
#10628=AXIS2_PLACEMENT_3D('',#16541,#13406,#13407);
#10629=AXIS2_PLACEMENT_3D('',#16542,#13408,#13409);
#10630=AXIS2_PLACEMENT_3D('',#16543,#13410,#13411);
#10631=AXIS2_PLACEMENT_3D('',#16544,#13412,#13413);
#10632=AXIS2_PLACEMENT_3D('',#16545,#13414,#13415);
#10633=AXIS2_PLACEMENT_3D('',#16546,#13416,#13417);
#10634=AXIS2_PLACEMENT_3D('',#16547,#13418,#13419);
#10635=AXIS2_PLACEMENT_3D('',#16548,#13420,#13421);
#10636=AXIS2_PLACEMENT_3D('',#16549,#13422,#13423);
#10637=AXIS2_PLACEMENT_3D('',#16550,#13424,#13425);
#10638=AXIS2_PLACEMENT_3D('',#16551,#13426,#13427);
#10639=AXIS2_PLACEMENT_3D('',#16552,#13428,#13429);
#10640=AXIS2_PLACEMENT_3D('',#16553,#13430,#13431);
#10641=AXIS2_PLACEMENT_3D('',#16554,#13432,#13433);
#10642=AXIS2_PLACEMENT_3D('',#16555,#13434,#13435);
#10643=AXIS2_PLACEMENT_3D('',#16556,#13436,#13437);
#10644=AXIS2_PLACEMENT_3D('',#16557,#13438,#13439);
#10645=AXIS2_PLACEMENT_3D('',#16558,#13440,#13441);
#10646=AXIS2_PLACEMENT_3D('',#16559,#13442,#13443);
#10647=AXIS2_PLACEMENT_3D('',#16560,#13444,#13445);
#10648=AXIS2_PLACEMENT_3D('',#16561,#13446,#13447);
#10649=AXIS2_PLACEMENT_3D('',#16562,#13448,#13449);
#10650=AXIS2_PLACEMENT_3D('',#16563,#13450,#13451);
#10651=AXIS2_PLACEMENT_3D('',#16564,#13452,#13453);
#10652=AXIS2_PLACEMENT_3D('',#16565,#13454,#13455);
#10653=AXIS2_PLACEMENT_3D('',#16566,#13456,#13457);
#10654=AXIS2_PLACEMENT_3D('',#16567,#13458,#13459);
#10655=AXIS2_PLACEMENT_3D('',#16568,#13460,#13461);
#10656=AXIS2_PLACEMENT_3D('',#16569,#13462,#13463);
#10657=AXIS2_PLACEMENT_3D('',#16570,#13464,#13465);
#10658=AXIS2_PLACEMENT_3D('',#16571,#13466,#13467);
#10659=AXIS2_PLACEMENT_3D('',#16572,#13468,#13469);
#10660=AXIS2_PLACEMENT_3D('',#16573,#13470,#13471);
#10661=AXIS2_PLACEMENT_3D('',#16574,#13472,#13473);
#10662=AXIS2_PLACEMENT_3D('',#16575,#13474,#13475);
#10663=AXIS2_PLACEMENT_3D('',#16576,#13476,#13477);
#10664=AXIS2_PLACEMENT_3D('',#16577,#13478,#13479);
#10665=AXIS2_PLACEMENT_3D('',#16578,#13480,#13481);
#10666=AXIS2_PLACEMENT_3D('',#16579,#13482,#13483);
#10667=AXIS2_PLACEMENT_3D('',#16580,#13484,#13485);
#10668=AXIS2_PLACEMENT_3D('',#16581,#13486,#13487);
#10669=AXIS2_PLACEMENT_3D('',#16582,#13488,#13489);
#10670=AXIS2_PLACEMENT_3D('',#16583,#13490,#13491);
#10671=AXIS2_PLACEMENT_3D('',#16584,#13492,#13493);
#10672=AXIS2_PLACEMENT_3D('',#16585,#13494,#13495);
#10673=AXIS2_PLACEMENT_3D('',#16594,#13500,#13501);
#10674=AXIS2_PLACEMENT_3D('',#16600,#13505,#13506);
#10675=AXIS2_PLACEMENT_3D('',#16606,#13510,#13511);
#10676=AXIS2_PLACEMENT_3D('',#16612,#13515,#13516);
#10677=AXIS2_PLACEMENT_3D('',#16618,#13520,#13521);
#10678=AXIS2_PLACEMENT_3D('',#16621,#13524,#13525);
#10679=AXIS2_PLACEMENT_3D('',#16622,#13526,#13527);
#10680=AXIS2_PLACEMENT_3D('',#16624,#13528,#13529);
#10681=AXIS2_PLACEMENT_3D('',#16625,#13530,#13531);
#10682=AXIS2_PLACEMENT_3D('',#16627,#13532,#13533);
#10683=AXIS2_PLACEMENT_3D('',#16629,#13535,#13536);
#10684=AXIS2_PLACEMENT_3D('',#16631,#13537,#13538);
#10685=AXIS2_PLACEMENT_3D('',#16633,#13540,#13541);
#10686=AXIS2_PLACEMENT_3D('',#16635,#13542,#13543);
#10687=AXIS2_PLACEMENT_3D('',#16637,#13545,#13546);
#10688=AXIS2_PLACEMENT_3D('',#16638,#13547,#13548);
#10689=AXIS2_PLACEMENT_3D('',#16639,#13549,#13550);
#10690=AXIS2_PLACEMENT_3D('',#16640,#13551,#13552);
#10691=AXIS2_PLACEMENT_3D('',#16641,#13553,#13554);
#10692=AXIS2_PLACEMENT_3D('',#16642,#13555,#13556);
#10693=AXIS2_PLACEMENT_3D('',#16643,#13557,#13558);
#10694=AXIS2_PLACEMENT_3D('',#16644,#13559,#13560);
#10695=AXIS2_PLACEMENT_3D('',#16645,#13561,#13562);
#10696=AXIS2_PLACEMENT_3D('',#16646,#13563,#13564);
#10697=AXIS2_PLACEMENT_3D('',#16647,#13565,#13566);
#10698=AXIS2_PLACEMENT_3D('',#16648,#13567,#13568);
#10699=AXIS2_PLACEMENT_3D('',#16649,#13569,#13570);
#10700=AXIS2_PLACEMENT_3D('',#16650,#13571,#13572);
#10701=AXIS2_PLACEMENT_3D('',#16651,#13573,#13574);
#10702=AXIS2_PLACEMENT_3D('',#16652,#13575,#13576);
#10703=AXIS2_PLACEMENT_3D('',#16653,#13577,#13578);
#10704=AXIS2_PLACEMENT_3D('',#16654,#13579,#13580);
#10705=AXIS2_PLACEMENT_3D('',#16655,#13581,#13582);
#10706=AXIS2_PLACEMENT_3D('',#16656,#13583,#13584);
#10707=AXIS2_PLACEMENT_3D('',#16657,#13585,#13586);
#10708=AXIS2_PLACEMENT_3D('',#16658,#13587,#13588);
#10709=AXIS2_PLACEMENT_3D('',#16659,#13589,#13590);
#10710=AXIS2_PLACEMENT_3D('',#16660,#13591,#13592);
#10711=AXIS2_PLACEMENT_3D('',#16661,#13593,#13594);
#10712=AXIS2_PLACEMENT_3D('',#16662,#13595,#13596);
#10713=AXIS2_PLACEMENT_3D('',#16663,#13597,#13598);
#10714=AXIS2_PLACEMENT_3D('',#16664,#13599,#13600);
#10715=AXIS2_PLACEMENT_3D('',#16665,#13601,#13602);
#10716=AXIS2_PLACEMENT_3D('',#16666,#13603,#13604);
#10717=AXIS2_PLACEMENT_3D('',#16667,#13605,#13606);
#10718=AXIS2_PLACEMENT_3D('',#16668,#13607,#13608);
#10719=AXIS2_PLACEMENT_3D('',#16669,#13609,#13610);
#10720=AXIS2_PLACEMENT_3D('',#16670,#13611,#13612);
#10721=AXIS2_PLACEMENT_3D('',#16671,#13613,#13614);
#10722=AXIS2_PLACEMENT_3D('',#16672,#13615,#13616);
#10723=AXIS2_PLACEMENT_3D('',#16673,#13617,#13618);
#10724=AXIS2_PLACEMENT_3D('',#16674,#13619,#13620);
#10725=AXIS2_PLACEMENT_3D('',#16675,#13621,#13622);
#10726=AXIS2_PLACEMENT_3D('',#16676,#13623,#13624);
#10727=AXIS2_PLACEMENT_3D('',#16677,#13625,#13626);
#10728=AXIS2_PLACEMENT_3D('',#16678,#13627,#13628);
#10729=AXIS2_PLACEMENT_3D('',#16679,#13629,#13630);
#10730=AXIS2_PLACEMENT_3D('',#16680,#13631,#13632);
#10731=AXIS2_PLACEMENT_3D('',#16681,#13633,#13634);
#10732=AXIS2_PLACEMENT_3D('',#16682,#13635,#13636);
#10733=AXIS2_PLACEMENT_3D('',#16683,#13637,#13638);
#10734=AXIS2_PLACEMENT_3D('',#16684,#13639,#13640);
#10735=AXIS2_PLACEMENT_3D('',#16685,#13641,#13642);
#10736=AXIS2_PLACEMENT_3D('',#16686,#13643,#13644);
#10737=AXIS2_PLACEMENT_3D('',#16687,#13645,#13646);
#10738=AXIS2_PLACEMENT_3D('',#16688,#13647,#13648);
#10739=AXIS2_PLACEMENT_3D('',#16689,#13649,#13650);
#10740=AXIS2_PLACEMENT_3D('',#16690,#13651,#13652);
#10741=AXIS2_PLACEMENT_3D('',#16691,#13653,#13654);
#10742=AXIS2_PLACEMENT_3D('',#16692,#13655,#13656);
#10743=AXIS2_PLACEMENT_3D('',#16693,#13657,#13658);
#10744=AXIS2_PLACEMENT_3D('',#16694,#13659,#13660);
#10745=AXIS2_PLACEMENT_3D('',#16695,#13661,#13662);
#10746=AXIS2_PLACEMENT_3D('',#16696,#13663,#13664);
#10747=AXIS2_PLACEMENT_3D('',#16697,#13665,#13666);
#10748=AXIS2_PLACEMENT_3D('',#16698,#13667,#13668);
#10749=AXIS2_PLACEMENT_3D('',#16699,#13669,#13670);
#10750=AXIS2_PLACEMENT_3D('',#16700,#13671,#13672);
#10751=AXIS2_PLACEMENT_3D('',#16701,#13673,#13674);
#10752=DIRECTION('axis',(0.,0.,1.));
#10753=DIRECTION('refdir',(1.,0.,0.));
#10754=DIRECTION('axis',(0.,0.,1.));
#10755=DIRECTION('refdir',(1.,0.,0.));
#10756=DIRECTION('axis',(0.,0.,1.));
#10757=DIRECTION('refdir',(1.,0.,0.));
#10758=DIRECTION('center_axis',(0.,0.,1.));
#10759=DIRECTION('ref_axis',(1.,0.,0.));
#10760=DIRECTION('center_axis',(0.,0.,1.));
#10761=DIRECTION('ref_axis',(1.,0.,0.));
#10762=DIRECTION('',(0.,0.,1.));
#10763=DIRECTION('center_axis',(0.,0.,-1.));
#10764=DIRECTION('ref_axis',(1.,0.,0.));
#10765=DIRECTION('center_axis',(0.,0.,1.));
#10766=DIRECTION('ref_axis',(1.,0.,0.));
#10767=DIRECTION('center_axis',(0.,0.,1.));
#10768=DIRECTION('ref_axis',(1.,0.,0.));
#10769=DIRECTION('',(0.,0.,1.));
#10770=DIRECTION('center_axis',(0.,0.,-1.));
#10771=DIRECTION('ref_axis',(1.,0.,0.));
#10772=DIRECTION('center_axis',(0.,0.,1.));
#10773=DIRECTION('ref_axis',(1.,0.,0.));
#10774=DIRECTION('center_axis',(0.,0.,1.));
#10775=DIRECTION('ref_axis',(1.,0.,0.));
#10776=DIRECTION('',(0.,0.,1.));
#10777=DIRECTION('center_axis',(0.,0.,-1.));
#10778=DIRECTION('ref_axis',(1.,0.,0.));
#10779=DIRECTION('center_axis',(0.,0.,1.));
#10780=DIRECTION('ref_axis',(1.,0.,0.));
#10781=DIRECTION('center_axis',(0.,0.,1.));
#10782=DIRECTION('ref_axis',(1.,0.,0.));
#10783=DIRECTION('',(0.,0.,1.));
#10784=DIRECTION('center_axis',(0.,0.,-1.));
#10785=DIRECTION('ref_axis',(1.,0.,0.));
#10786=DIRECTION('center_axis',(0.,0.,1.));
#10787=DIRECTION('ref_axis',(1.,0.,0.));
#10788=DIRECTION('center_axis',(0.,0.,1.));
#10789=DIRECTION('ref_axis',(1.,0.,0.));
#10790=DIRECTION('',(0.,0.,1.));
#10791=DIRECTION('center_axis',(0.,0.,-1.));
#10792=DIRECTION('ref_axis',(1.,0.,0.));
#10793=DIRECTION('center_axis',(0.,0.,1.));
#10794=DIRECTION('ref_axis',(1.,0.,0.));
#10795=DIRECTION('center_axis',(0.,0.,1.));
#10796=DIRECTION('ref_axis',(1.,0.,0.));
#10797=DIRECTION('',(0.,0.,1.));
#10798=DIRECTION('center_axis',(0.,0.,-1.));
#10799=DIRECTION('ref_axis',(1.,0.,0.));
#10800=DIRECTION('center_axis',(0.,0.,1.));
#10801=DIRECTION('ref_axis',(1.,0.,0.));
#10802=DIRECTION('center_axis',(0.,0.,1.));
#10803=DIRECTION('ref_axis',(1.,0.,0.));
#10804=DIRECTION('',(0.,0.,1.));
#10805=DIRECTION('center_axis',(0.,0.,-1.));
#10806=DIRECTION('ref_axis',(1.,0.,0.));
#10807=DIRECTION('center_axis',(0.,0.,1.));
#10808=DIRECTION('ref_axis',(1.,0.,0.));
#10809=DIRECTION('center_axis',(0.,0.,1.));
#10810=DIRECTION('ref_axis',(1.,0.,0.));
#10811=DIRECTION('',(0.,0.,1.));
#10812=DIRECTION('center_axis',(0.,0.,-1.));
#10813=DIRECTION('ref_axis',(1.,0.,0.));
#10814=DIRECTION('center_axis',(0.,0.,1.));
#10815=DIRECTION('ref_axis',(1.,0.,0.));
#10816=DIRECTION('center_axis',(0.,0.,1.));
#10817=DIRECTION('ref_axis',(1.,0.,0.));
#10818=DIRECTION('',(0.,0.,1.));
#10819=DIRECTION('center_axis',(0.,0.,-1.));
#10820=DIRECTION('ref_axis',(1.,0.,0.));
#10821=DIRECTION('center_axis',(0.,0.,1.));
#10822=DIRECTION('ref_axis',(1.,0.,0.));
#10823=DIRECTION('center_axis',(0.,0.,1.));
#10824=DIRECTION('ref_axis',(1.,0.,0.));
#10825=DIRECTION('',(0.,0.,1.));
#10826=DIRECTION('center_axis',(0.,0.,-1.));
#10827=DIRECTION('ref_axis',(1.,0.,0.));
#10828=DIRECTION('center_axis',(0.,0.,1.));
#10829=DIRECTION('ref_axis',(1.,0.,0.));
#10830=DIRECTION('center_axis',(0.,0.,1.));
#10831=DIRECTION('ref_axis',(1.,0.,0.));
#10832=DIRECTION('',(0.,0.,1.));
#10833=DIRECTION('center_axis',(0.,0.,-1.));
#10834=DIRECTION('ref_axis',(1.,0.,0.));
#10835=DIRECTION('center_axis',(0.,0.,1.));
#10836=DIRECTION('ref_axis',(1.,0.,0.));
#10837=DIRECTION('center_axis',(0.,0.,1.));
#10838=DIRECTION('ref_axis',(1.,0.,0.));
#10839=DIRECTION('',(0.,0.,1.));
#10840=DIRECTION('center_axis',(0.,0.,-1.));
#10841=DIRECTION('ref_axis',(1.,0.,0.));
#10842=DIRECTION('center_axis',(0.,1.,0.));
#10843=DIRECTION('ref_axis',(-1.,0.,0.));
#10844=DIRECTION('',(-1.,0.,0.));
#10845=DIRECTION('',(0.,0.,1.));
#10846=DIRECTION('',(-1.,0.,0.));
#10847=DIRECTION('',(0.,0.,1.));
#10848=DIRECTION('center_axis',(1.,0.,0.));
#10849=DIRECTION('ref_axis',(0.,1.,0.));
#10850=DIRECTION('',(0.,1.,0.));
#10851=DIRECTION('',(0.,1.,0.));
#10852=DIRECTION('',(0.,0.,1.));
#10853=DIRECTION('center_axis',(0.,-1.,0.));
#10854=DIRECTION('ref_axis',(1.,0.,0.));
#10855=DIRECTION('',(1.,0.,0.));
#10856=DIRECTION('',(1.,0.,0.));
#10857=DIRECTION('',(0.,0.,1.));
#10858=DIRECTION('center_axis',(-1.,0.,0.));
#10859=DIRECTION('ref_axis',(0.,-1.,0.));
#10860=DIRECTION('',(0.,-1.,0.));
#10861=DIRECTION('',(0.,-1.,0.));
#10862=DIRECTION('center_axis',(0.,0.,1.));
#10863=DIRECTION('ref_axis',(1.,0.,0.));
#10864=DIRECTION('center_axis',(0.,0.,1.));
#10865=DIRECTION('ref_axis',(1.,0.,0.));
#10866=DIRECTION('axis',(0.,0.,1.));
#10867=DIRECTION('refdir',(1.,0.,0.));
#10868=DIRECTION('center_axis',(0.,1.,0.));
#10869=DIRECTION('ref_axis',(-1.,0.,0.));
#10870=DIRECTION('',(-1.,0.,0.));
#10871=DIRECTION('',(0.,0.,1.));
#10872=DIRECTION('',(-1.,0.,0.));
#10873=DIRECTION('',(0.,0.,1.));
#10874=DIRECTION('center_axis',(1.,0.,0.));
#10875=DIRECTION('ref_axis',(0.,1.,0.));
#10876=DIRECTION('',(0.,1.,0.));
#10877=DIRECTION('',(0.,1.,0.));
#10878=DIRECTION('',(0.,0.,1.));
#10879=DIRECTION('center_axis',(0.,-1.,0.));
#10880=DIRECTION('ref_axis',(1.,0.,0.));
#10881=DIRECTION('',(1.,0.,0.));
#10882=DIRECTION('',(1.,0.,0.));
#10883=DIRECTION('',(0.,0.,1.));
#10884=DIRECTION('center_axis',(-1.,0.,0.));
#10885=DIRECTION('ref_axis',(0.,-1.,0.));
#10886=DIRECTION('',(0.,-1.,0.));
#10887=DIRECTION('',(0.,-1.,0.));
#10888=DIRECTION('center_axis',(0.,0.,1.));
#10889=DIRECTION('ref_axis',(1.,0.,0.));
#10890=DIRECTION('center_axis',(0.,0.,1.));
#10891=DIRECTION('ref_axis',(1.,0.,0.));
#10892=DIRECTION('axis',(0.,0.,1.));
#10893=DIRECTION('refdir',(1.,0.,0.));
#10894=DIRECTION('center_axis',(0.,1.,0.));
#10895=DIRECTION('ref_axis',(-1.,0.,0.));
#10896=DIRECTION('',(-1.,0.,0.));
#10897=DIRECTION('',(0.,0.,1.));
#10898=DIRECTION('',(-1.,0.,0.));
#10899=DIRECTION('',(0.,0.,1.));
#10900=DIRECTION('center_axis',(1.,0.,0.));
#10901=DIRECTION('ref_axis',(0.,1.,0.));
#10902=DIRECTION('',(0.,1.,0.));
#10903=DIRECTION('',(0.,1.,0.));
#10904=DIRECTION('',(0.,0.,1.));
#10905=DIRECTION('center_axis',(0.,-1.,0.));
#10906=DIRECTION('ref_axis',(1.,0.,0.));
#10907=DIRECTION('',(1.,0.,0.));
#10908=DIRECTION('',(1.,0.,0.));
#10909=DIRECTION('',(0.,0.,1.));
#10910=DIRECTION('center_axis',(-1.,0.,0.));
#10911=DIRECTION('ref_axis',(0.,-1.,0.));
#10912=DIRECTION('',(0.,-1.,0.));
#10913=DIRECTION('',(0.,-1.,0.));
#10914=DIRECTION('center_axis',(0.,0.,1.));
#10915=DIRECTION('ref_axis',(1.,0.,0.));
#10916=DIRECTION('center_axis',(0.,0.,1.));
#10917=DIRECTION('ref_axis',(1.,0.,0.));
#10918=DIRECTION('axis',(0.,0.,1.));
#10919=DIRECTION('refdir',(1.,0.,0.));
#10920=DIRECTION('center_axis',(0.,0.,1.));
#10921=DIRECTION('ref_axis',(1.,0.,0.));
#10922=DIRECTION('',(0.,0.,1.));
#10923=DIRECTION('center_axis',(0.,0.,1.));
#10924=DIRECTION('ref_axis',(1.,0.,0.));
#10925=DIRECTION('',(0.,0.,1.));
#10926=DIRECTION('center_axis',(0.,0.,-1.));
#10927=DIRECTION('ref_axis',(1.,0.,0.));
#10928=DIRECTION('center_axis',(0.,0.,1.));
#10929=DIRECTION('ref_axis',(1.,0.,0.));
#10930=DIRECTION('',(0.,0.,1.));
#10931=DIRECTION('center_axis',(0.,0.,1.));
#10932=DIRECTION('ref_axis',(1.,0.,0.));
#10933=DIRECTION('',(0.,0.,1.));
#10934=DIRECTION('center_axis',(0.,0.,-1.));
#10935=DIRECTION('ref_axis',(1.,0.,0.));
#10936=DIRECTION('center_axis',(0.,0.,1.));
#10937=DIRECTION('ref_axis',(1.,0.,0.));
#10938=DIRECTION('',(1.,0.,0.));
#10939=DIRECTION('center_axis',(0.,0.,1.));
#10940=DIRECTION('ref_axis',(1.,0.,0.));
#10941=DIRECTION('center_axis',(0.,0.,1.));
#10942=DIRECTION('ref_axis',(1.,0.,0.));
#10943=DIRECTION('center_axis',(0.,0.,1.));
#10944=DIRECTION('ref_axis',(1.,0.,0.));
#10945=DIRECTION('',(0.,0.,1.));
#10946=DIRECTION('center_axis',(0.,0.,-1.));
#10947=DIRECTION('ref_axis',(1.,0.,0.));
#10948=DIRECTION('center_axis',(0.,0.,1.));
#10949=DIRECTION('ref_axis',(1.,0.,0.));
#10950=DIRECTION('',(-1.,0.,0.));
#10951=DIRECTION('center_axis',(0.,0.,1.));
#10952=DIRECTION('ref_axis',(1.,0.,0.));
#10953=DIRECTION('center_axis',(0.,0.,-1.));
#10954=DIRECTION('ref_axis',(1.,0.,0.));
#10955=DIRECTION('',(0.,0.,1.));
#10956=DIRECTION('center_axis',(0.,0.,1.));
#10957=DIRECTION('ref_axis',(1.,0.,0.));
#10958=DIRECTION('center_axis',(0.,0.,1.));
#10959=DIRECTION('ref_axis',(1.,0.,0.));
#10960=DIRECTION('center_axis',(0.,0.,1.));
#10961=DIRECTION('ref_axis',(1.,0.,0.));
#10962=DIRECTION('center_axis',(0.,0.,1.));
#10963=DIRECTION('ref_axis',(1.,0.,0.));
#10964=DIRECTION('center_axis',(0.,0.,-1.));
#10965=DIRECTION('ref_axis',(1.,0.,0.));
#10966=DIRECTION('',(0.,0.,1.));
#10967=DIRECTION('center_axis',(0.,0.,1.));
#10968=DIRECTION('ref_axis',(1.,0.,0.));
#10969=DIRECTION('center_axis',(0.,0.,1.));
#10970=DIRECTION('ref_axis',(1.,0.,0.));
#10971=DIRECTION('center_axis',(0.,0.,1.));
#10972=DIRECTION('ref_axis',(1.,0.,0.));
#10973=DIRECTION('center_axis',(0.,0.,1.));
#10974=DIRECTION('ref_axis',(1.,0.,0.));
#10975=DIRECTION('',(0.,-1.,0.));
#10976=DIRECTION('',(1.,0.,0.));
#10977=DIRECTION('',(1.,0.,0.));
#10978=DIRECTION('',(0.,1.,0.));
#10979=DIRECTION('',(-1.,0.,0.));
#10980=DIRECTION('',(-1.,0.,0.));
#10981=DIRECTION('center_axis',(0.,0.,1.));
#10982=DIRECTION('ref_axis',(1.,0.,0.));
#10983=DIRECTION('center_axis',(0.,0.,1.));
#10984=DIRECTION('ref_axis',(1.,0.,0.));
#10985=DIRECTION('',(0.,0.,1.));
#10986=DIRECTION('center_axis',(0.,0.,1.));
#10987=DIRECTION('ref_axis',(1.,0.,0.));
#10988=DIRECTION('center_axis',(0.,0.,1.));
#10989=DIRECTION('ref_axis',(1.,0.,0.));
#10990=DIRECTION('',(0.,0.,1.));
#10991=DIRECTION('center_axis',(1.,0.,0.));
#10992=DIRECTION('ref_axis',(0.,0.,-1.));
#10993=DIRECTION('center_axis',(1.,0.,0.));
#10994=DIRECTION('ref_axis',(0.,0.,-1.));
#10995=DIRECTION('',(1.,0.,0.));
#10996=DIRECTION('',(1.,0.,0.));
#10997=DIRECTION('center_axis',(-1.,0.,0.));
#10998=DIRECTION('ref_axis',(0.,0.,-1.));
#10999=DIRECTION('center_axis',(0.,1.,0.));
#11000=DIRECTION('ref_axis',(-1.,0.,0.));
#11001=DIRECTION('',(-1.,0.,0.));
#11002=DIRECTION('',(0.,0.,1.));
#11003=DIRECTION('',(0.,0.,1.));
#11004=DIRECTION('center_axis',(1.,0.,0.));
#11005=DIRECTION('ref_axis',(0.,1.,0.));
#11006=DIRECTION('',(0.,1.,0.));
#11007=DIRECTION('',(0.,0.,1.));
#11008=DIRECTION('center_axis',(0.,-1.,0.));
#11009=DIRECTION('ref_axis',(1.,0.,0.));
#11010=DIRECTION('',(1.,0.,0.));
#11011=DIRECTION('',(0.,0.,1.));
#11012=DIRECTION('center_axis',(-1.,0.,0.));
#11013=DIRECTION('ref_axis',(0.,-1.,0.));
#11014=DIRECTION('',(0.,-1.,0.));
#11015=DIRECTION('center_axis',(0.,0.,1.));
#11016=DIRECTION('ref_axis',(1.,0.,0.));
#11017=DIRECTION('axis',(0.,0.,1.));
#11018=DIRECTION('refdir',(1.,0.,0.));
#11019=DIRECTION('center_axis',(0.,0.,1.));
#11020=DIRECTION('ref_axis',(1.,0.,0.));
#11021=DIRECTION('',(0.,0.,1.));
#11022=DIRECTION('center_axis',(0.,0.,1.));
#11023=DIRECTION('ref_axis',(1.,0.,0.));
#11024=DIRECTION('',(0.,0.,1.));
#11025=DIRECTION('center_axis',(0.,0.,-1.));
#11026=DIRECTION('ref_axis',(1.,0.,0.));
#11027=DIRECTION('center_axis',(0.,0.,1.));
#11028=DIRECTION('ref_axis',(1.,0.,0.));
#11029=DIRECTION('',(0.,0.,1.));
#11030=DIRECTION('center_axis',(0.,0.,1.));
#11031=DIRECTION('ref_axis',(1.,0.,0.));
#11032=DIRECTION('',(0.,0.,1.));
#11033=DIRECTION('center_axis',(0.,0.,-1.));
#11034=DIRECTION('ref_axis',(1.,0.,0.));
#11035=DIRECTION('center_axis',(0.,0.,1.));
#11036=DIRECTION('ref_axis',(1.,0.,0.));
#11037=DIRECTION('',(1.,0.,0.));
#11038=DIRECTION('center_axis',(0.,0.,1.));
#11039=DIRECTION('ref_axis',(1.,0.,0.));
#11040=DIRECTION('center_axis',(0.,0.,1.));
#11041=DIRECTION('ref_axis',(1.,0.,0.));
#11042=DIRECTION('center_axis',(0.,0.,1.));
#11043=DIRECTION('ref_axis',(1.,0.,0.));
#11044=DIRECTION('',(0.,0.,1.));
#11045=DIRECTION('center_axis',(0.,0.,-1.));
#11046=DIRECTION('ref_axis',(1.,0.,0.));
#11047=DIRECTION('center_axis',(0.,0.,1.));
#11048=DIRECTION('ref_axis',(1.,0.,0.));
#11049=DIRECTION('',(-1.,0.,0.));
#11050=DIRECTION('center_axis',(0.,0.,1.));
#11051=DIRECTION('ref_axis',(1.,0.,0.));
#11052=DIRECTION('center_axis',(0.,0.,-1.));
#11053=DIRECTION('ref_axis',(1.,0.,0.));
#11054=DIRECTION('',(0.,0.,1.));
#11055=DIRECTION('center_axis',(0.,0.,1.));
#11056=DIRECTION('ref_axis',(1.,0.,0.));
#11057=DIRECTION('center_axis',(0.,0.,1.));
#11058=DIRECTION('ref_axis',(1.,0.,0.));
#11059=DIRECTION('center_axis',(0.,0.,1.));
#11060=DIRECTION('ref_axis',(1.,0.,0.));
#11061=DIRECTION('center_axis',(0.,0.,1.));
#11062=DIRECTION('ref_axis',(1.,0.,0.));
#11063=DIRECTION('center_axis',(0.,0.,-1.));
#11064=DIRECTION('ref_axis',(1.,0.,0.));
#11065=DIRECTION('',(0.,0.,1.));
#11066=DIRECTION('center_axis',(0.,0.,1.));
#11067=DIRECTION('ref_axis',(1.,0.,0.));
#11068=DIRECTION('center_axis',(0.,0.,1.));
#11069=DIRECTION('ref_axis',(1.,0.,0.));
#11070=DIRECTION('center_axis',(0.,0.,1.));
#11071=DIRECTION('ref_axis',(1.,0.,0.));
#11072=DIRECTION('center_axis',(0.,0.,1.));
#11073=DIRECTION('ref_axis',(1.,0.,0.));
#11074=DIRECTION('',(0.,-1.,0.));
#11075=DIRECTION('',(1.,0.,0.));
#11076=DIRECTION('',(1.,0.,0.));
#11077=DIRECTION('',(0.,1.,0.));
#11078=DIRECTION('',(-1.,0.,0.));
#11079=DIRECTION('',(-1.,0.,0.));
#11080=DIRECTION('center_axis',(0.,0.,1.));
#11081=DIRECTION('ref_axis',(1.,0.,0.));
#11082=DIRECTION('center_axis',(0.,0.,1.));
#11083=DIRECTION('ref_axis',(1.,0.,0.));
#11084=DIRECTION('',(0.,0.,1.));
#11085=DIRECTION('center_axis',(0.,0.,1.));
#11086=DIRECTION('ref_axis',(1.,0.,0.));
#11087=DIRECTION('center_axis',(0.,0.,1.));
#11088=DIRECTION('ref_axis',(1.,0.,0.));
#11089=DIRECTION('',(0.,0.,1.));
#11090=DIRECTION('center_axis',(1.,0.,0.));
#11091=DIRECTION('ref_axis',(0.,0.,-1.));
#11092=DIRECTION('center_axis',(1.,0.,0.));
#11093=DIRECTION('ref_axis',(0.,0.,-1.));
#11094=DIRECTION('',(1.,0.,0.));
#11095=DIRECTION('',(1.,0.,0.));
#11096=DIRECTION('center_axis',(-1.,0.,0.));
#11097=DIRECTION('ref_axis',(0.,0.,-1.));
#11098=DIRECTION('center_axis',(0.,1.,0.));
#11099=DIRECTION('ref_axis',(-1.,0.,0.));
#11100=DIRECTION('',(-1.,0.,0.));
#11101=DIRECTION('',(0.,0.,1.));
#11102=DIRECTION('',(0.,0.,1.));
#11103=DIRECTION('center_axis',(1.,0.,0.));
#11104=DIRECTION('ref_axis',(0.,1.,0.));
#11105=DIRECTION('',(0.,1.,0.));
#11106=DIRECTION('',(0.,0.,1.));
#11107=DIRECTION('center_axis',(0.,-1.,0.));
#11108=DIRECTION('ref_axis',(1.,0.,0.));
#11109=DIRECTION('',(1.,0.,0.));
#11110=DIRECTION('',(0.,0.,1.));
#11111=DIRECTION('center_axis',(-1.,0.,0.));
#11112=DIRECTION('ref_axis',(0.,-1.,0.));
#11113=DIRECTION('',(0.,-1.,0.));
#11114=DIRECTION('center_axis',(0.,0.,1.));
#11115=DIRECTION('ref_axis',(1.,0.,0.));
#11116=DIRECTION('axis',(0.,0.,1.));
#11117=DIRECTION('refdir',(1.,0.,0.));
#11118=DIRECTION('center_axis',(0.,0.,1.));
#11119=DIRECTION('ref_axis',(1.,0.,0.));
#11120=DIRECTION('',(0.,0.,1.));
#11121=DIRECTION('center_axis',(0.,0.,1.));
#11122=DIRECTION('ref_axis',(1.,0.,0.));
#11123=DIRECTION('',(0.,0.,1.));
#11124=DIRECTION('center_axis',(0.,0.,-1.));
#11125=DIRECTION('ref_axis',(1.,0.,0.));
#11126=DIRECTION('center_axis',(0.,0.,1.));
#11127=DIRECTION('ref_axis',(1.,0.,0.));
#11128=DIRECTION('',(0.,0.,1.));
#11129=DIRECTION('center_axis',(0.,0.,1.));
#11130=DIRECTION('ref_axis',(1.,0.,0.));
#11131=DIRECTION('',(0.,0.,1.));
#11132=DIRECTION('center_axis',(0.,0.,-1.));
#11133=DIRECTION('ref_axis',(1.,0.,0.));
#11134=DIRECTION('center_axis',(0.,0.,1.));
#11135=DIRECTION('ref_axis',(1.,0.,0.));
#11136=DIRECTION('',(1.,0.,0.));
#11137=DIRECTION('center_axis',(0.,0.,1.));
#11138=DIRECTION('ref_axis',(1.,0.,0.));
#11139=DIRECTION('center_axis',(0.,0.,1.));
#11140=DIRECTION('ref_axis',(1.,0.,0.));
#11141=DIRECTION('center_axis',(0.,0.,1.));
#11142=DIRECTION('ref_axis',(1.,0.,0.));
#11143=DIRECTION('',(0.,0.,1.));
#11144=DIRECTION('center_axis',(0.,0.,-1.));
#11145=DIRECTION('ref_axis',(1.,0.,0.));
#11146=DIRECTION('center_axis',(0.,0.,1.));
#11147=DIRECTION('ref_axis',(1.,0.,0.));
#11148=DIRECTION('',(-1.,0.,0.));
#11149=DIRECTION('center_axis',(0.,0.,1.));
#11150=DIRECTION('ref_axis',(1.,0.,0.));
#11151=DIRECTION('center_axis',(0.,0.,-1.));
#11152=DIRECTION('ref_axis',(1.,0.,0.));
#11153=DIRECTION('',(0.,0.,1.));
#11154=DIRECTION('center_axis',(0.,0.,1.));
#11155=DIRECTION('ref_axis',(1.,0.,0.));
#11156=DIRECTION('center_axis',(0.,0.,1.));
#11157=DIRECTION('ref_axis',(1.,0.,0.));
#11158=DIRECTION('center_axis',(0.,0.,1.));
#11159=DIRECTION('ref_axis',(1.,0.,0.));
#11160=DIRECTION('center_axis',(0.,0.,1.));
#11161=DIRECTION('ref_axis',(1.,0.,0.));
#11162=DIRECTION('center_axis',(0.,0.,-1.));
#11163=DIRECTION('ref_axis',(1.,0.,0.));
#11164=DIRECTION('',(0.,0.,1.));
#11165=DIRECTION('center_axis',(0.,0.,1.));
#11166=DIRECTION('ref_axis',(1.,0.,0.));
#11167=DIRECTION('center_axis',(0.,0.,1.));
#11168=DIRECTION('ref_axis',(1.,0.,0.));
#11169=DIRECTION('center_axis',(0.,0.,1.));
#11170=DIRECTION('ref_axis',(1.,0.,0.));
#11171=DIRECTION('center_axis',(0.,0.,1.));
#11172=DIRECTION('ref_axis',(1.,0.,0.));
#11173=DIRECTION('',(0.,-1.,0.));
#11174=DIRECTION('',(1.,0.,0.));
#11175=DIRECTION('',(1.,0.,0.));
#11176=DIRECTION('',(0.,1.,0.));
#11177=DIRECTION('',(-1.,0.,0.));
#11178=DIRECTION('',(-1.,0.,0.));
#11179=DIRECTION('center_axis',(0.,0.,1.));
#11180=DIRECTION('ref_axis',(1.,0.,0.));
#11181=DIRECTION('center_axis',(0.,0.,1.));
#11182=DIRECTION('ref_axis',(1.,0.,0.));
#11183=DIRECTION('',(0.,0.,1.));
#11184=DIRECTION('center_axis',(0.,0.,1.));
#11185=DIRECTION('ref_axis',(1.,0.,0.));
#11186=DIRECTION('center_axis',(0.,0.,1.));
#11187=DIRECTION('ref_axis',(1.,0.,0.));
#11188=DIRECTION('',(0.,0.,1.));
#11189=DIRECTION('center_axis',(1.,0.,0.));
#11190=DIRECTION('ref_axis',(0.,0.,-1.));
#11191=DIRECTION('center_axis',(1.,0.,0.));
#11192=DIRECTION('ref_axis',(0.,0.,-1.));
#11193=DIRECTION('',(1.,0.,0.));
#11194=DIRECTION('',(1.,0.,0.));
#11195=DIRECTION('center_axis',(-1.,0.,0.));
#11196=DIRECTION('ref_axis',(0.,0.,-1.));
#11197=DIRECTION('center_axis',(0.,1.,0.));
#11198=DIRECTION('ref_axis',(-1.,0.,0.));
#11199=DIRECTION('',(-1.,0.,0.));
#11200=DIRECTION('',(0.,0.,1.));
#11201=DIRECTION('',(0.,0.,1.));
#11202=DIRECTION('center_axis',(1.,0.,0.));
#11203=DIRECTION('ref_axis',(0.,1.,0.));
#11204=DIRECTION('',(0.,1.,0.));
#11205=DIRECTION('',(0.,0.,1.));
#11206=DIRECTION('center_axis',(0.,-1.,0.));
#11207=DIRECTION('ref_axis',(1.,0.,0.));
#11208=DIRECTION('',(1.,0.,0.));
#11209=DIRECTION('',(0.,0.,1.));
#11210=DIRECTION('center_axis',(-1.,0.,0.));
#11211=DIRECTION('ref_axis',(0.,-1.,0.));
#11212=DIRECTION('',(0.,-1.,0.));
#11213=DIRECTION('center_axis',(0.,0.,1.));
#11214=DIRECTION('ref_axis',(1.,0.,0.));
#11215=DIRECTION('axis',(0.,0.,1.));
#11216=DIRECTION('refdir',(1.,0.,0.));
#11217=DIRECTION('center_axis',(0.,0.,1.));
#11218=DIRECTION('ref_axis',(1.,0.,0.));
#11219=DIRECTION('',(0.,0.,1.));
#11220=DIRECTION('center_axis',(0.,0.,1.));
#11221=DIRECTION('ref_axis',(1.,0.,0.));
#11222=DIRECTION('',(0.,0.,1.));
#11223=DIRECTION('center_axis',(0.,0.,-1.));
#11224=DIRECTION('ref_axis',(1.,0.,0.));
#11225=DIRECTION('center_axis',(0.,0.,1.));
#11226=DIRECTION('ref_axis',(1.,0.,0.));
#11227=DIRECTION('',(0.,0.,1.));
#11228=DIRECTION('center_axis',(0.,0.,1.));
#11229=DIRECTION('ref_axis',(1.,0.,0.));
#11230=DIRECTION('',(0.,0.,1.));
#11231=DIRECTION('center_axis',(0.,0.,-1.));
#11232=DIRECTION('ref_axis',(1.,0.,0.));
#11233=DIRECTION('center_axis',(0.,0.,1.));
#11234=DIRECTION('ref_axis',(1.,0.,0.));
#11235=DIRECTION('',(1.,0.,0.));
#11236=DIRECTION('center_axis',(0.,0.,1.));
#11237=DIRECTION('ref_axis',(1.,0.,0.));
#11238=DIRECTION('center_axis',(0.,0.,1.));
#11239=DIRECTION('ref_axis',(1.,0.,0.));
#11240=DIRECTION('center_axis',(0.,0.,1.));
#11241=DIRECTION('ref_axis',(1.,0.,0.));
#11242=DIRECTION('',(0.,0.,1.));
#11243=DIRECTION('center_axis',(0.,0.,-1.));
#11244=DIRECTION('ref_axis',(1.,0.,0.));
#11245=DIRECTION('center_axis',(0.,0.,1.));
#11246=DIRECTION('ref_axis',(1.,0.,0.));
#11247=DIRECTION('',(-1.,0.,0.));
#11248=DIRECTION('center_axis',(0.,0.,1.));
#11249=DIRECTION('ref_axis',(1.,0.,0.));
#11250=DIRECTION('center_axis',(0.,0.,-1.));
#11251=DIRECTION('ref_axis',(1.,0.,0.));
#11252=DIRECTION('',(0.,0.,1.));
#11253=DIRECTION('center_axis',(0.,0.,1.));
#11254=DIRECTION('ref_axis',(1.,0.,0.));
#11255=DIRECTION('center_axis',(0.,0.,1.));
#11256=DIRECTION('ref_axis',(1.,0.,0.));
#11257=DIRECTION('center_axis',(0.,0.,1.));
#11258=DIRECTION('ref_axis',(1.,0.,0.));
#11259=DIRECTION('center_axis',(0.,0.,1.));
#11260=DIRECTION('ref_axis',(1.,0.,0.));
#11261=DIRECTION('center_axis',(0.,0.,-1.));
#11262=DIRECTION('ref_axis',(1.,0.,0.));
#11263=DIRECTION('',(0.,0.,1.));
#11264=DIRECTION('center_axis',(0.,0.,1.));
#11265=DIRECTION('ref_axis',(1.,0.,0.));
#11266=DIRECTION('center_axis',(0.,0.,1.));
#11267=DIRECTION('ref_axis',(1.,0.,0.));
#11268=DIRECTION('center_axis',(0.,0.,1.));
#11269=DIRECTION('ref_axis',(1.,0.,0.));
#11270=DIRECTION('center_axis',(0.,0.,1.));
#11271=DIRECTION('ref_axis',(1.,0.,0.));
#11272=DIRECTION('',(0.,-1.,0.));
#11273=DIRECTION('',(1.,0.,0.));
#11274=DIRECTION('',(1.,0.,0.));
#11275=DIRECTION('',(0.,1.,0.));
#11276=DIRECTION('',(-1.,0.,0.));
#11277=DIRECTION('',(-1.,0.,0.));
#11278=DIRECTION('center_axis',(0.,0.,1.));
#11279=DIRECTION('ref_axis',(1.,0.,0.));
#11280=DIRECTION('center_axis',(0.,0.,1.));
#11281=DIRECTION('ref_axis',(1.,0.,0.));
#11282=DIRECTION('',(0.,0.,1.));
#11283=DIRECTION('center_axis',(0.,0.,1.));
#11284=DIRECTION('ref_axis',(1.,0.,0.));
#11285=DIRECTION('center_axis',(0.,0.,1.));
#11286=DIRECTION('ref_axis',(1.,0.,0.));
#11287=DIRECTION('',(0.,0.,1.));
#11288=DIRECTION('center_axis',(1.,0.,0.));
#11289=DIRECTION('ref_axis',(0.,0.,-1.));
#11290=DIRECTION('center_axis',(1.,0.,0.));
#11291=DIRECTION('ref_axis',(0.,0.,-1.));
#11292=DIRECTION('',(1.,0.,0.));
#11293=DIRECTION('',(1.,0.,0.));
#11294=DIRECTION('center_axis',(-1.,0.,0.));
#11295=DIRECTION('ref_axis',(0.,0.,-1.));
#11296=DIRECTION('center_axis',(0.,1.,0.));
#11297=DIRECTION('ref_axis',(-1.,0.,0.));
#11298=DIRECTION('',(-1.,0.,0.));
#11299=DIRECTION('',(0.,0.,1.));
#11300=DIRECTION('',(0.,0.,1.));
#11301=DIRECTION('center_axis',(1.,0.,0.));
#11302=DIRECTION('ref_axis',(0.,1.,0.));
#11303=DIRECTION('',(0.,1.,0.));
#11304=DIRECTION('',(0.,0.,1.));
#11305=DIRECTION('center_axis',(0.,-1.,0.));
#11306=DIRECTION('ref_axis',(1.,0.,0.));
#11307=DIRECTION('',(1.,0.,0.));
#11308=DIRECTION('',(0.,0.,1.));
#11309=DIRECTION('center_axis',(-1.,0.,0.));
#11310=DIRECTION('ref_axis',(0.,-1.,0.));
#11311=DIRECTION('',(0.,-1.,0.));
#11312=DIRECTION('center_axis',(0.,0.,1.));
#11313=DIRECTION('ref_axis',(1.,0.,0.));
#11314=DIRECTION('axis',(0.,0.,1.));
#11315=DIRECTION('refdir',(1.,0.,0.));
#11316=DIRECTION('center_axis',(1.,0.,0.));
#11317=DIRECTION('ref_axis',(0.,0.,-1.));
#11318=DIRECTION('center_axis',(1.,0.,0.));
#11319=DIRECTION('ref_axis',(0.,0.,-1.));
#11320=DIRECTION('',(1.,0.,0.));
#11321=DIRECTION('center_axis',(-1.,0.,0.));
#11322=DIRECTION('ref_axis',(0.,0.,-1.));
#11323=DIRECTION('center_axis',(1.,0.,0.));
#11324=DIRECTION('ref_axis',(0.,0.,-1.));
#11325=DIRECTION('center_axis',(1.,0.,0.));
#11326=DIRECTION('ref_axis',(0.,0.,-1.));
#11327=DIRECTION('',(1.,0.,0.));
#11328=DIRECTION('center_axis',(-1.,0.,0.));
#11329=DIRECTION('ref_axis',(0.,0.,-1.));
#11330=DIRECTION('center_axis',(1.,0.,0.));
#11331=DIRECTION('ref_axis',(0.,0.,-1.));
#11332=DIRECTION('center_axis',(1.,0.,0.));
#11333=DIRECTION('ref_axis',(0.,0.,-1.));
#11334=DIRECTION('',(1.,0.,0.));
#11335=DIRECTION('center_axis',(-1.,0.,0.));
#11336=DIRECTION('ref_axis',(0.,0.,-1.));
#11337=DIRECTION('center_axis',(1.,0.,0.));
#11338=DIRECTION('ref_axis',(0.,0.,-1.));
#11339=DIRECTION('center_axis',(1.,0.,0.));
#11340=DIRECTION('ref_axis',(0.,0.,-1.));
#11341=DIRECTION('',(1.,0.,0.));
#11342=DIRECTION('center_axis',(-1.,0.,0.));
#11343=DIRECTION('ref_axis',(0.,0.,-1.));
#11344=DIRECTION('center_axis',(0.,0.,1.));
#11345=DIRECTION('ref_axis',(1.,0.,0.));
#11346=DIRECTION('center_axis',(0.,0.,1.));
#11347=DIRECTION('ref_axis',(1.,0.,0.));
#11348=DIRECTION('',(0.,0.,1.));
#11349=DIRECTION('center_axis',(0.,0.,-1.));
#11350=DIRECTION('ref_axis',(1.,0.,0.));
#11351=DIRECTION('center_axis',(0.,0.,1.));
#11352=DIRECTION('ref_axis',(1.,0.,0.));
#11353=DIRECTION('center_axis',(0.,0.,1.));
#11354=DIRECTION('ref_axis',(1.,0.,0.));
#11355=DIRECTION('',(0.,0.,1.));
#11356=DIRECTION('center_axis',(0.,0.,-1.));
#11357=DIRECTION('ref_axis',(1.,0.,0.));
#11358=DIRECTION('center_axis',(1.,0.,0.));
#11359=DIRECTION('ref_axis',(0.,0.,-1.));
#11360=DIRECTION('center_axis',(1.,0.,0.));
#11361=DIRECTION('ref_axis',(0.,0.,-1.));
#11362=DIRECTION('',(1.,0.,0.));
#11363=DIRECTION('center_axis',(-1.,0.,0.));
#11364=DIRECTION('ref_axis',(0.,0.,-1.));
#11365=DIRECTION('center_axis',(0.,0.,1.));
#11366=DIRECTION('ref_axis',(0.,-1.,0.));
#11367=DIRECTION('',(-1.,0.,0.));
#11368=DIRECTION('',(0.,-1.,0.));
#11369=DIRECTION('',(1.,0.,0.));
#11370=DIRECTION('',(0.,-1.,0.));
#11371=DIRECTION('center_axis',(0.,0.,1.));
#11372=DIRECTION('ref_axis',(0.,-1.,0.));
#11373=DIRECTION('',(1.,0.,0.));
#11374=DIRECTION('',(0.,-1.,0.));
#11375=DIRECTION('',(1.,0.,0.));
#11376=DIRECTION('',(0.,-1.,0.));
#11377=DIRECTION('center_axis',(0.,1.,0.));
#11378=DIRECTION('ref_axis',(0.,0.,1.));
#11379=DIRECTION('',(0.,0.,1.));
#11380=DIRECTION('',(0.,0.,1.));
#11381=DIRECTION('',(1.,0.,0.));
#11382=DIRECTION('center_axis',(0.,-1.,0.));
#11383=DIRECTION('ref_axis',(0.,0.,-1.));
#11384=DIRECTION('',(0.,0.,-1.));
#11385=DIRECTION('',(1.,0.,0.));
#11386=DIRECTION('',(0.,0.,-1.));
#11387=DIRECTION('center_axis',(0.,-1.,0.));
#11388=DIRECTION('ref_axis',(1.,0.,0.));
#11389=DIRECTION('',(0.,0.,1.));
#11390=DIRECTION('',(1.,0.,0.));
#11391=DIRECTION('',(0.,0.,1.));
#11392=DIRECTION('center_axis',(1.,0.,0.));
#11393=DIRECTION('ref_axis',(0.,1.,0.));
#11394=DIRECTION('',(0.,0.,1.));
#11395=DIRECTION('',(0.,1.,0.));
#11396=DIRECTION('',(0.,1.,0.));
#11397=DIRECTION('center_axis',(0.,1.,0.));
#11398=DIRECTION('ref_axis',(-1.,0.,0.));
#11399=DIRECTION('',(0.,0.,1.));
#11400=DIRECTION('',(-1.,0.,0.));
#11401=DIRECTION('center_axis',(-1.,0.,0.));
#11402=DIRECTION('ref_axis',(0.,-1.,0.));
#11403=DIRECTION('',(0.,-1.,0.));
#11404=DIRECTION('',(0.,-1.,0.));
#11405=DIRECTION('center_axis',(0.,0.,1.));
#11406=DIRECTION('ref_axis',(1.,0.,0.));
#11407=DIRECTION('center_axis',(0.,0.,1.));
#11408=DIRECTION('ref_axis',(1.,0.,0.));
#11409=DIRECTION('axis',(0.,0.,1.));
#11410=DIRECTION('refdir',(1.,0.,0.));
#11411=DIRECTION('center_axis',(1.,0.,0.));
#11412=DIRECTION('ref_axis',(0.,0.,-1.));
#11413=DIRECTION('center_axis',(1.,0.,0.));
#11414=DIRECTION('ref_axis',(0.,0.,-1.));
#11415=DIRECTION('',(1.,0.,0.));
#11416=DIRECTION('center_axis',(-1.,0.,0.));
#11417=DIRECTION('ref_axis',(0.,0.,-1.));
#11418=DIRECTION('center_axis',(1.,0.,0.));
#11419=DIRECTION('ref_axis',(0.,0.,-1.));
#11420=DIRECTION('center_axis',(1.,0.,0.));
#11421=DIRECTION('ref_axis',(0.,0.,-1.));
#11422=DIRECTION('',(1.,0.,0.));
#11423=DIRECTION('center_axis',(-1.,0.,0.));
#11424=DIRECTION('ref_axis',(0.,0.,-1.));
#11425=DIRECTION('center_axis',(1.,0.,0.));
#11426=DIRECTION('ref_axis',(0.,0.,-1.));
#11427=DIRECTION('center_axis',(1.,0.,0.));
#11428=DIRECTION('ref_axis',(0.,0.,-1.));
#11429=DIRECTION('',(1.,0.,0.));
#11430=DIRECTION('center_axis',(-1.,0.,0.));
#11431=DIRECTION('ref_axis',(0.,0.,-1.));
#11432=DIRECTION('center_axis',(1.,0.,0.));
#11433=DIRECTION('ref_axis',(0.,0.,-1.));
#11434=DIRECTION('center_axis',(1.,0.,0.));
#11435=DIRECTION('ref_axis',(0.,0.,-1.));
#11436=DIRECTION('',(1.,0.,0.));
#11437=DIRECTION('center_axis',(-1.,0.,0.));
#11438=DIRECTION('ref_axis',(0.,0.,-1.));
#11439=DIRECTION('center_axis',(1.,0.,0.));
#11440=DIRECTION('ref_axis',(0.,0.,-1.));
#11441=DIRECTION('center_axis',(1.,0.,0.));
#11442=DIRECTION('ref_axis',(0.,0.,-1.));
#11443=DIRECTION('',(-1.,0.,0.));
#11444=DIRECTION('center_axis',(-1.,0.,0.));
#11445=DIRECTION('ref_axis',(0.,0.,-1.));
#11446=DIRECTION('center_axis',(1.,0.,0.));
#11447=DIRECTION('ref_axis',(0.,0.,-1.));
#11448=DIRECTION('center_axis',(-1.,0.,0.));
#11449=DIRECTION('ref_axis',(0.,0.,-1.));
#11450=DIRECTION('center_axis',(1.,0.,0.));
#11451=DIRECTION('ref_axis',(0.,0.,-1.));
#11452=DIRECTION('',(-1.,0.,0.));
#11453=DIRECTION('center_axis',(-1.,0.,0.));
#11454=DIRECTION('ref_axis',(0.,0.,-1.));
#11455=DIRECTION('center_axis',(1.,0.,0.));
#11456=DIRECTION('ref_axis',(0.,0.,-1.));
#11457=DIRECTION('center_axis',(1.,0.,0.));
#11458=DIRECTION('ref_axis',(0.,0.,-1.));
#11459=DIRECTION('',(-1.,0.,0.));
#11460=DIRECTION('center_axis',(1.,0.,0.));
#11461=DIRECTION('ref_axis',(0.,0.,-1.));
#11462=DIRECTION('center_axis',(1.,0.,0.));
#11463=DIRECTION('ref_axis',(0.,0.,-1.));
#11464=DIRECTION('center_axis',(1.,0.,0.));
#11465=DIRECTION('ref_axis',(0.,0.,-1.));
#11466=DIRECTION('axis',(0.,0.,1.));
#11467=DIRECTION('refdir',(1.,0.,0.));
#11468=DIRECTION('center_axis',(1.,0.,0.));
#11469=DIRECTION('ref_axis',(0.,0.,-1.));
#11470=DIRECTION('center_axis',(1.,0.,0.));
#11471=DIRECTION('ref_axis',(0.,0.,-1.));
#11472=DIRECTION('',(1.,0.,0.));
#11473=DIRECTION('center_axis',(-1.,0.,0.));
#11474=DIRECTION('ref_axis',(0.,0.,-1.));
#11475=DIRECTION('center_axis',(1.,0.,0.));
#11476=DIRECTION('ref_axis',(0.,0.,-1.));
#11477=DIRECTION('center_axis',(1.,0.,0.));
#11478=DIRECTION('ref_axis',(0.,0.,-1.));
#11479=DIRECTION('',(1.,0.,0.));
#11480=DIRECTION('center_axis',(-1.,0.,0.));
#11481=DIRECTION('ref_axis',(0.,0.,-1.));
#11482=DIRECTION('center_axis',(1.,0.,0.));
#11483=DIRECTION('ref_axis',(0.,0.,-1.));
#11484=DIRECTION('center_axis',(1.,0.,0.));
#11485=DIRECTION('ref_axis',(0.,0.,-1.));
#11486=DIRECTION('',(1.,0.,0.));
#11487=DIRECTION('center_axis',(-1.,0.,0.));
#11488=DIRECTION('ref_axis',(0.,0.,-1.));
#11489=DIRECTION('center_axis',(1.,0.,0.));
#11490=DIRECTION('ref_axis',(0.,0.,-1.));
#11491=DIRECTION('center_axis',(1.,0.,0.));
#11492=DIRECTION('ref_axis',(0.,0.,-1.));
#11493=DIRECTION('',(1.,0.,0.));
#11494=DIRECTION('center_axis',(-1.,0.,0.));
#11495=DIRECTION('ref_axis',(0.,0.,-1.));
#11496=DIRECTION('center_axis',(1.,0.,0.));
#11497=DIRECTION('ref_axis',(0.,0.,-1.));
#11498=DIRECTION('center_axis',(1.,0.,0.));
#11499=DIRECTION('ref_axis',(0.,0.,-1.));
#11500=DIRECTION('',(-1.,0.,0.));
#11501=DIRECTION('center_axis',(1.,0.,0.));
#11502=DIRECTION('ref_axis',(0.,0.,-1.));
#11503=DIRECTION('center_axis',(1.,0.,0.));
#11504=DIRECTION('ref_axis',(0.,0.,-1.));
#11505=DIRECTION('center_axis',(-1.,0.,0.));
#11506=DIRECTION('ref_axis',(0.,0.,-1.));
#11507=DIRECTION('center_axis',(1.,0.,0.));
#11508=DIRECTION('ref_axis',(0.,0.,-1.));
#11509=DIRECTION('center_axis',(-1.,0.,0.));
#11510=DIRECTION('ref_axis',(0.,0.,-1.));
#11511=DIRECTION('',(-1.,0.,0.));
#11512=DIRECTION('center_axis',(1.,0.,0.));
#11513=DIRECTION('ref_axis',(0.,0.,-1.));
#11514=DIRECTION('center_axis',(1.,0.,0.));
#11515=DIRECTION('ref_axis',(0.,0.,-1.));
#11516=DIRECTION('',(-1.,0.,0.));
#11517=DIRECTION('center_axis',(1.,0.,0.));
#11518=DIRECTION('ref_axis',(0.,0.,-1.));
#11519=DIRECTION('center_axis',(1.,0.,0.));
#11520=DIRECTION('ref_axis',(0.,0.,-1.));
#11521=DIRECTION('center_axis',(1.,0.,0.));
#11522=DIRECTION('ref_axis',(0.,0.,-1.));
#11523=DIRECTION('axis',(0.,0.,1.));
#11524=DIRECTION('refdir',(1.,0.,0.));
#11525=DIRECTION('center_axis',(1.,0.,0.));
#11526=DIRECTION('ref_axis',(0.,0.,-1.));
#11527=DIRECTION('center_axis',(1.,0.,0.));
#11528=DIRECTION('ref_axis',(0.,0.,-1.));
#11529=DIRECTION('',(1.,0.,0.));
#11530=DIRECTION('center_axis',(-1.,0.,0.));
#11531=DIRECTION('ref_axis',(0.,0.,-1.));
#11532=DIRECTION('center_axis',(1.,0.,0.));
#11533=DIRECTION('ref_axis',(0.,0.,-1.));
#11534=DIRECTION('center_axis',(1.,0.,0.));
#11535=DIRECTION('ref_axis',(0.,0.,-1.));
#11536=DIRECTION('',(1.,0.,0.));
#11537=DIRECTION('center_axis',(-1.,0.,0.));
#11538=DIRECTION('ref_axis',(0.,0.,-1.));
#11539=DIRECTION('center_axis',(1.,0.,0.));
#11540=DIRECTION('ref_axis',(0.,0.,-1.));
#11541=DIRECTION('center_axis',(1.,0.,0.));
#11542=DIRECTION('ref_axis',(0.,0.,-1.));
#11543=DIRECTION('',(1.,0.,0.));
#11544=DIRECTION('center_axis',(-1.,0.,0.));
#11545=DIRECTION('ref_axis',(0.,0.,-1.));
#11546=DIRECTION('center_axis',(1.,0.,0.));
#11547=DIRECTION('ref_axis',(0.,0.,-1.));
#11548=DIRECTION('center_axis',(1.,0.,0.));
#11549=DIRECTION('ref_axis',(0.,0.,-1.));
#11550=DIRECTION('',(1.,0.,0.));
#11551=DIRECTION('center_axis',(-1.,0.,0.));
#11552=DIRECTION('ref_axis',(0.,0.,-1.));
#11553=DIRECTION('center_axis',(0.,0.,1.));
#11554=DIRECTION('ref_axis',(1.,0.,0.));
#11555=DIRECTION('center_axis',(0.,0.,1.));
#11556=DIRECTION('ref_axis',(1.,0.,0.));
#11557=DIRECTION('',(0.,0.,1.));
#11558=DIRECTION('center_axis',(0.,0.,-1.));
#11559=DIRECTION('ref_axis',(1.,0.,0.));
#11560=DIRECTION('center_axis',(0.,0.,1.));
#11561=DIRECTION('ref_axis',(1.,0.,0.));
#11562=DIRECTION('center_axis',(0.,0.,1.));
#11563=DIRECTION('ref_axis',(1.,0.,0.));
#11564=DIRECTION('',(0.,0.,1.));
#11565=DIRECTION('center_axis',(0.,0.,-1.));
#11566=DIRECTION('ref_axis',(1.,0.,0.));
#11567=DIRECTION('center_axis',(1.,0.,0.));
#11568=DIRECTION('ref_axis',(0.,0.,-1.));
#11569=DIRECTION('center_axis',(1.,0.,0.));
#11570=DIRECTION('ref_axis',(0.,0.,-1.));
#11571=DIRECTION('',(1.,0.,0.));
#11572=DIRECTION('center_axis',(-1.,0.,0.));
#11573=DIRECTION('ref_axis',(0.,0.,-1.));
#11574=DIRECTION('center_axis',(0.,0.,1.));
#11575=DIRECTION('ref_axis',(0.,-1.,0.));
#11576=DIRECTION('',(-1.,0.,0.));
#11577=DIRECTION('',(0.,-1.,0.));
#11578=DIRECTION('',(1.,0.,0.));
#11579=DIRECTION('',(0.,-1.,0.));
#11580=DIRECTION('center_axis',(0.,0.,1.));
#11581=DIRECTION('ref_axis',(0.,-1.,0.));
#11582=DIRECTION('',(1.,0.,0.));
#11583=DIRECTION('',(0.,-1.,0.));
#11584=DIRECTION('',(1.,0.,0.));
#11585=DIRECTION('',(0.,-1.,0.));
#11586=DIRECTION('center_axis',(0.,1.,0.));
#11587=DIRECTION('ref_axis',(0.,0.,1.));
#11588=DIRECTION('',(0.,0.,1.));
#11589=DIRECTION('',(0.,0.,1.));
#11590=DIRECTION('',(1.,0.,0.));
#11591=DIRECTION('center_axis',(0.,-1.,0.));
#11592=DIRECTION('ref_axis',(0.,0.,-1.));
#11593=DIRECTION('',(0.,0.,-1.));
#11594=DIRECTION('',(1.,0.,0.));
#11595=DIRECTION('',(0.,0.,-1.));
#11596=DIRECTION('center_axis',(0.,-1.,0.));
#11597=DIRECTION('ref_axis',(1.,0.,0.));
#11598=DIRECTION('',(0.,0.,1.));
#11599=DIRECTION('',(1.,0.,0.));
#11600=DIRECTION('',(0.,0.,1.));
#11601=DIRECTION('center_axis',(1.,0.,0.));
#11602=DIRECTION('ref_axis',(0.,1.,0.));
#11603=DIRECTION('',(0.,0.,1.));
#11604=DIRECTION('',(0.,1.,0.));
#11605=DIRECTION('',(0.,1.,0.));
#11606=DIRECTION('center_axis',(0.,1.,0.));
#11607=DIRECTION('ref_axis',(-1.,0.,0.));
#11608=DIRECTION('',(0.,0.,1.));
#11609=DIRECTION('',(-1.,0.,0.));
#11610=DIRECTION('center_axis',(-1.,0.,0.));
#11611=DIRECTION('ref_axis',(0.,-1.,0.));
#11612=DIRECTION('',(0.,-1.,0.));
#11613=DIRECTION('',(0.,-1.,0.));
#11614=DIRECTION('center_axis',(0.,0.,1.));
#11615=DIRECTION('ref_axis',(1.,0.,0.));
#11616=DIRECTION('center_axis',(0.,0.,1.));
#11617=DIRECTION('ref_axis',(1.,0.,0.));
#11618=DIRECTION('axis',(0.,0.,1.));
#11619=DIRECTION('refdir',(1.,0.,0.));
#11620=DIRECTION('center_axis',(1.,0.,0.));
#11621=DIRECTION('ref_axis',(0.,0.,-1.));
#11622=DIRECTION('center_axis',(1.,0.,0.));
#11623=DIRECTION('ref_axis',(0.,0.,-1.));
#11624=DIRECTION('',(1.,0.,0.));
#11625=DIRECTION('center_axis',(-1.,0.,0.));
#11626=DIRECTION('ref_axis',(0.,0.,-1.));
#11627=DIRECTION('center_axis',(1.,0.,0.));
#11628=DIRECTION('ref_axis',(0.,0.,-1.));
#11629=DIRECTION('center_axis',(1.,0.,0.));
#11630=DIRECTION('ref_axis',(0.,0.,-1.));
#11631=DIRECTION('',(1.,0.,0.));
#11632=DIRECTION('center_axis',(-1.,0.,0.));
#11633=DIRECTION('ref_axis',(0.,0.,-1.));
#11634=DIRECTION('center_axis',(1.,0.,0.));
#11635=DIRECTION('ref_axis',(0.,0.,-1.));
#11636=DIRECTION('center_axis',(1.,0.,0.));
#11637=DIRECTION('ref_axis',(0.,0.,-1.));
#11638=DIRECTION('',(1.,0.,0.));
#11639=DIRECTION('center_axis',(-1.,0.,0.));
#11640=DIRECTION('ref_axis',(0.,0.,-1.));
#11641=DIRECTION('center_axis',(1.,0.,0.));
#11642=DIRECTION('ref_axis',(0.,0.,-1.));
#11643=DIRECTION('center_axis',(1.,0.,0.));
#11644=DIRECTION('ref_axis',(0.,0.,-1.));
#11645=DIRECTION('',(1.,0.,0.));
#11646=DIRECTION('center_axis',(-1.,0.,0.));
#11647=DIRECTION('ref_axis',(0.,0.,-1.));
#11648=DIRECTION('center_axis',(1.,0.,0.));
#11649=DIRECTION('ref_axis',(0.,0.,-1.));
#11650=DIRECTION('center_axis',(1.,0.,0.));
#11651=DIRECTION('ref_axis',(0.,0.,-1.));
#11652=DIRECTION('',(-1.,0.,0.));
#11653=DIRECTION('center_axis',(-1.,0.,0.));
#11654=DIRECTION('ref_axis',(0.,0.,-1.));
#11655=DIRECTION('center_axis',(1.,0.,0.));
#11656=DIRECTION('ref_axis',(0.,0.,-1.));
#11657=DIRECTION('center_axis',(-1.,0.,0.));
#11658=DIRECTION('ref_axis',(0.,0.,-1.));
#11659=DIRECTION('center_axis',(1.,0.,0.));
#11660=DIRECTION('ref_axis',(0.,0.,-1.));
#11661=DIRECTION('',(-1.,0.,0.));
#11662=DIRECTION('center_axis',(-1.,0.,0.));
#11663=DIRECTION('ref_axis',(0.,0.,-1.));
#11664=DIRECTION('center_axis',(1.,0.,0.));
#11665=DIRECTION('ref_axis',(0.,0.,-1.));
#11666=DIRECTION('center_axis',(1.,0.,0.));
#11667=DIRECTION('ref_axis',(0.,0.,-1.));
#11668=DIRECTION('',(-1.,0.,0.));
#11669=DIRECTION('center_axis',(1.,0.,0.));
#11670=DIRECTION('ref_axis',(0.,0.,-1.));
#11671=DIRECTION('center_axis',(1.,0.,0.));
#11672=DIRECTION('ref_axis',(0.,0.,-1.));
#11673=DIRECTION('center_axis',(1.,0.,0.));
#11674=DIRECTION('ref_axis',(0.,0.,-1.));
#11675=DIRECTION('axis',(0.,0.,1.));
#11676=DIRECTION('refdir',(1.,0.,0.));
#11677=DIRECTION('center_axis',(1.,0.,0.));
#11678=DIRECTION('ref_axis',(0.,0.,-1.));
#11679=DIRECTION('center_axis',(1.,0.,0.));
#11680=DIRECTION('ref_axis',(0.,0.,-1.));
#11681=DIRECTION('',(1.,0.,0.));
#11682=DIRECTION('center_axis',(-1.,0.,0.));
#11683=DIRECTION('ref_axis',(0.,0.,-1.));
#11684=DIRECTION('center_axis',(1.,0.,0.));
#11685=DIRECTION('ref_axis',(0.,0.,-1.));
#11686=DIRECTION('center_axis',(1.,0.,0.));
#11687=DIRECTION('ref_axis',(0.,0.,-1.));
#11688=DIRECTION('',(1.,0.,0.));
#11689=DIRECTION('center_axis',(-1.,0.,0.));
#11690=DIRECTION('ref_axis',(0.,0.,-1.));
#11691=DIRECTION('center_axis',(1.,0.,0.));
#11692=DIRECTION('ref_axis',(0.,0.,-1.));
#11693=DIRECTION('center_axis',(1.,0.,0.));
#11694=DIRECTION('ref_axis',(0.,0.,-1.));
#11695=DIRECTION('',(1.,0.,0.));
#11696=DIRECTION('center_axis',(-1.,0.,0.));
#11697=DIRECTION('ref_axis',(0.,0.,-1.));
#11698=DIRECTION('center_axis',(1.,0.,0.));
#11699=DIRECTION('ref_axis',(0.,0.,-1.));
#11700=DIRECTION('center_axis',(1.,0.,0.));
#11701=DIRECTION('ref_axis',(0.,0.,-1.));
#11702=DIRECTION('',(1.,0.,0.));
#11703=DIRECTION('center_axis',(-1.,0.,0.));
#11704=DIRECTION('ref_axis',(0.,0.,-1.));
#11705=DIRECTION('center_axis',(1.,0.,0.));
#11706=DIRECTION('ref_axis',(0.,0.,-1.));
#11707=DIRECTION('center_axis',(1.,0.,0.));
#11708=DIRECTION('ref_axis',(0.,0.,-1.));
#11709=DIRECTION('',(-1.,0.,0.));
#11710=DIRECTION('center_axis',(1.,0.,0.));
#11711=DIRECTION('ref_axis',(0.,0.,-1.));
#11712=DIRECTION('center_axis',(1.,0.,0.));
#11713=DIRECTION('ref_axis',(0.,0.,-1.));
#11714=DIRECTION('center_axis',(-1.,0.,0.));
#11715=DIRECTION('ref_axis',(0.,0.,-1.));
#11716=DIRECTION('center_axis',(1.,0.,0.));
#11717=DIRECTION('ref_axis',(0.,0.,-1.));
#11718=DIRECTION('center_axis',(-1.,0.,0.));
#11719=DIRECTION('ref_axis',(0.,0.,-1.));
#11720=DIRECTION('',(-1.,0.,0.));
#11721=DIRECTION('center_axis',(1.,0.,0.));
#11722=DIRECTION('ref_axis',(0.,0.,-1.));
#11723=DIRECTION('center_axis',(1.,0.,0.));
#11724=DIRECTION('ref_axis',(0.,0.,-1.));
#11725=DIRECTION('',(-1.,0.,0.));
#11726=DIRECTION('center_axis',(1.,0.,0.));
#11727=DIRECTION('ref_axis',(0.,0.,-1.));
#11728=DIRECTION('center_axis',(1.,0.,0.));
#11729=DIRECTION('ref_axis',(0.,0.,-1.));
#11730=DIRECTION('center_axis',(1.,0.,0.));
#11731=DIRECTION('ref_axis',(0.,0.,-1.));
#11732=DIRECTION('axis',(0.,0.,1.));
#11733=DIRECTION('refdir',(1.,0.,0.));
#11734=DIRECTION('center_axis',(1.,0.,0.));
#11735=DIRECTION('ref_axis',(0.,0.,-1.));
#11736=DIRECTION('center_axis',(-1.,0.,0.));
#11737=DIRECTION('ref_axis',(0.,0.,-1.));
#11738=DIRECTION('',(-0.707106781186548,8.65956056235493E-17,-0.707106781186547));
#11739=DIRECTION('center_axis',(1.,0.,0.));
#11740=DIRECTION('ref_axis',(0.,0.,-1.));
#11741=DIRECTION('center_axis',(1.,0.,0.));
#11742=DIRECTION('ref_axis',(0.,0.,-1.));
#11743=DIRECTION('center_axis',(1.,0.,0.));
#11744=DIRECTION('ref_axis',(0.,0.,-1.));
#11745=DIRECTION('',(-1.,0.,0.));
#11746=DIRECTION('center_axis',(1.,0.,0.));
#11747=DIRECTION('ref_axis',(0.,0.,-1.));
#11748=DIRECTION('center_axis',(-1.,0.,0.));
#11749=DIRECTION('ref_axis',(0.,0.,-1.));
#11750=DIRECTION('center_axis',(-1.,0.,0.));
#11751=DIRECTION('ref_axis',(0.,0.,-1.));
#11752=DIRECTION('',(-0.707106781186553,-8.65956056235487E-17,0.707106781186542));
#11753=DIRECTION('center_axis',(1.,0.,0.));
#11754=DIRECTION('ref_axis',(0.,0.,-1.));
#11755=DIRECTION('axis',(0.,0.,1.));
#11756=DIRECTION('refdir',(1.,0.,0.));
#11757=DIRECTION('axis',(0.,0.,1.));
#11758=DIRECTION('refdir',(1.,0.,0.));
#11759=DIRECTION('center_axis',(0.,-1.,0.));
#11760=DIRECTION('ref_axis',(0.,0.,-1.));
#11761=DIRECTION('center_axis',(0.,-1.,0.));
#11762=DIRECTION('ref_axis',(1.,0.,0.));
#11763=DIRECTION('center_axis',(0.,-1.,0.));
#11764=DIRECTION('ref_axis',(1.,0.,0.));
#11765=DIRECTION('center_axis',(1.,0.,1.22464679914735E-16));
#11766=DIRECTION('ref_axis',(-1.22464679914735E-16,0.,1.));
#11767=DIRECTION('center_axis',(0.,1.,0.));
#11768=DIRECTION('ref_axis',(1.,0.,0.));
#11769=DIRECTION('center_axis',(0.,1.,0.));
#11770=DIRECTION('ref_axis',(1.,0.,0.));
#11771=DIRECTION('center_axis',(0.,-1.,0.));
#11772=DIRECTION('ref_axis',(1.,0.,0.));
#11773=DIRECTION('',(0.,1.,0.));
#11774=DIRECTION('center_axis',(0.,-1.,0.));
#11775=DIRECTION('ref_axis',(1.,0.,0.));
#11776=DIRECTION('center_axis',(0.,-1.,0.));
#11777=DIRECTION('ref_axis',(1.,0.,0.));
#11778=DIRECTION('center_axis',(0.,-1.,0.));
#11779=DIRECTION('ref_axis',(1.,0.,0.));
#11780=DIRECTION('',(0.,1.,0.));
#11781=DIRECTION('center_axis',(0.,-1.,0.));
#11782=DIRECTION('ref_axis',(1.,0.,0.));
#11783=DIRECTION('center_axis',(0.,1.,0.));
#11784=DIRECTION('ref_axis',(1.,0.,0.));
#11785=DIRECTION('',(-0.707106781186548,0.707106781186547,-8.65956056235493E-17));
#11786=DIRECTION('center_axis',(0.,-1.,0.));
#11787=DIRECTION('ref_axis',(1.,0.,0.));
#11788=DIRECTION('center_axis',(0.,1.,0.));
#11789=DIRECTION('ref_axis',(0.,0.,1.));
#11790=DIRECTION('center_axis',(0.,-1.,0.));
#11791=DIRECTION('ref_axis',(1.,0.,0.));
#11792=DIRECTION('center_axis',(0.,-1.,0.));
#11793=DIRECTION('ref_axis',(1.,0.,0.));
#11794=DIRECTION('',(0.,1.,0.));
#11795=DIRECTION('center_axis',(0.,-1.,0.));
#11796=DIRECTION('ref_axis',(0.,0.,-1.));
#11797=DIRECTION('center_axis',(0.,-1.,0.));
#11798=DIRECTION('ref_axis',(1.,0.,0.));
#11799=DIRECTION('center_axis',(0.,-1.,0.));
#11800=DIRECTION('ref_axis',(1.,0.,0.));
#11801=DIRECTION('',(0.707106781186548,0.707106781186547,8.65956056235493E-17));
#11802=DIRECTION('axis',(0.,0.,1.));
#11803=DIRECTION('refdir',(1.,0.,0.));
#11804=DIRECTION('center_axis',(0.,-1.,0.));
#11805=DIRECTION('ref_axis',(0.,0.,-1.));
#11806=DIRECTION('center_axis',(0.,-1.,0.));
#11807=DIRECTION('ref_axis',(1.,0.,0.));
#11808=DIRECTION('center_axis',(0.,-1.,0.));
#11809=DIRECTION('ref_axis',(1.,0.,0.));
#11810=DIRECTION('center_axis',(1.,0.,1.22464679914735E-16));
#11811=DIRECTION('ref_axis',(-1.22464679914735E-16,0.,1.));
#11812=DIRECTION('center_axis',(0.,1.,0.));
#11813=DIRECTION('ref_axis',(1.,0.,0.));
#11814=DIRECTION('center_axis',(0.,1.,0.));
#11815=DIRECTION('ref_axis',(1.,0.,0.));
#11816=DIRECTION('center_axis',(0.,-1.,0.));
#11817=DIRECTION('ref_axis',(1.,0.,0.));
#11818=DIRECTION('center_axis',(0.,-1.,0.));
#11819=DIRECTION('ref_axis',(1.,0.,0.));
#11820=DIRECTION('',(0.,1.,0.));
#11821=DIRECTION('center_axis',(0.,1.,0.));
#11822=DIRECTION('ref_axis',(0.,0.,1.));
#11823=DIRECTION('center_axis',(0.,-1.,0.));
#11824=DIRECTION('ref_axis',(1.,0.,0.));
#11825=DIRECTION('center_axis',(0.,-1.,0.));
#11826=DIRECTION('ref_axis',(1.,0.,0.));
#11827=DIRECTION('center_axis',(0.,-1.,0.));
#11828=DIRECTION('ref_axis',(1.,0.,0.));
#11829=DIRECTION('center_axis',(0.,-1.,0.));
#11830=DIRECTION('ref_axis',(1.,0.,0.));
#11831=DIRECTION('',(0.707106781186548,0.707106781186547,8.65956056235494E-17));
#11832=DIRECTION('center_axis',(0.,-1.,0.));
#11833=DIRECTION('ref_axis',(1.,0.,0.));
#11834=DIRECTION('center_axis',(0.,-1.,0.));
#11835=DIRECTION('ref_axis',(1.,0.,0.));
#11836=DIRECTION('',(0.,1.,0.));
#11837=DIRECTION('center_axis',(0.,1.,0.));
#11838=DIRECTION('ref_axis',(1.,0.,0.));
#11839=DIRECTION('center_axis',(0.,-1.,0.));
#11840=DIRECTION('ref_axis',(1.,0.,0.));
#11841=DIRECTION('',(-0.707106781186548,0.707106781186547,-8.65956056235494E-17));
#11842=DIRECTION('center_axis',(0.,-1.,0.));
#11843=DIRECTION('ref_axis',(0.,0.,-1.));
#11844=DIRECTION('center_axis',(0.,-1.,0.));
#11845=DIRECTION('ref_axis',(1.,0.,0.));
#11846=DIRECTION('',(0.,1.,0.));
#11847=DIRECTION('axis',(0.,0.,1.));
#11848=DIRECTION('refdir',(1.,0.,0.));
#11849=DIRECTION('center_axis',(0.,0.,1.));
#11850=DIRECTION('ref_axis',(1.,0.,0.));
#11851=DIRECTION('center_axis',(1.22464679914735E-16,-1.,0.));
#11852=DIRECTION('ref_axis',(-1.,-1.22464679914735E-16,0.));
#11853=DIRECTION('center_axis',(0.78183148246803,0.,0.623489801858733));
#11854=DIRECTION('ref_axis',(0.623489801858734,0.,-0.78183148246803));
#11855=DIRECTION('center_axis',(7.63554790147315E-17,-1.,-9.57467422477103E-17));
#11856=DIRECTION('ref_axis',(-0.623489801858734,-1.22464679914735E-16,0.78183148246803));
#11857=DIRECTION('center_axis',(0.974927912181824,0.,-0.222520933956314));
#11858=DIRECTION('ref_axis',(-0.222520933956314,0.,-0.974927912181824));
#11859=DIRECTION('center_axis',(-2.7250954951288E-17,-1.,-1.19394234705288E-16));
#11860=DIRECTION('ref_axis',(0.222520933956314,-1.22464679914735E-16,0.974927912181824));
#11861=DIRECTION('center_axis',(0.433883739117558,0.,-0.900968867902419));
#11862=DIRECTION('ref_axis',(-0.900968867902419,0.,-0.433883739117558));
#11863=DIRECTION('center_axis',(-1.10336864020811E-16,-1.,-5.31354332312403E-17));
#11864=DIRECTION('ref_axis',(0.900968867902419,-1.22464679914735E-16,0.433883739117558));
#11865=DIRECTION('center_axis',(-0.433883739117558,0.,-0.900968867902419));
#11866=DIRECTION('ref_axis',(-0.900968867902419,0.,0.433883739117558));
#11867=DIRECTION('center_axis',(-1.10336864020811E-16,-1.,5.31354332312403E-17));
#11868=DIRECTION('ref_axis',(0.900968867902419,-1.22464679914735E-16,-0.433883739117558));
#11869=DIRECTION('center_axis',(-0.974927912181824,0.,-0.222520933956314));
#11870=DIRECTION('ref_axis',(-0.222520933956315,0.,0.974927912181824));
#11871=DIRECTION('center_axis',(-2.7250954951288E-17,-1.,1.19394234705288E-16));
#11872=DIRECTION('ref_axis',(0.222520933956315,-1.22464679914735E-16,-0.974927912181824));
#11873=DIRECTION('center_axis',(-0.78183148246803,0.,0.623489801858734));
#11874=DIRECTION('ref_axis',(0.623489801858733,0.,0.78183148246803));
#11875=DIRECTION('center_axis',(7.63554790147315E-17,-1.,9.57467422477103E-17));
#11876=DIRECTION('ref_axis',(-0.623489801858733,-1.22464679914735E-16,-0.78183148246803));
#11877=DIRECTION('axis',(0.,0.,1.));
#11878=DIRECTION('refdir',(1.,0.,0.));
#11879=DIRECTION('center_axis',(0.,0.,1.));
#11880=DIRECTION('ref_axis',(1.,0.,0.));
#11881=DIRECTION('center_axis',(0.,-1.,0.));
#11882=DIRECTION('ref_axis',(0.,0.,-1.));
#11883=DIRECTION('center_axis',(0.,-1.,0.));
#11884=DIRECTION('ref_axis',(0.,0.,-1.));
#11885=DIRECTION('center_axis',(0.,1.,0.));
#11886=DIRECTION('ref_axis',(1.,0.,0.));
#11887=DIRECTION('center_axis',(0.,1.,0.));
#11888=DIRECTION('ref_axis',(1.,0.,0.));
#11889=DIRECTION('center_axis',(0.,1.,0.));
#11890=DIRECTION('ref_axis',(1.,0.,0.));
#11891=DIRECTION('center_axis',(0.,1.,0.));
#11892=DIRECTION('ref_axis',(1.,0.,0.));
#11893=DIRECTION('',(0.,-1.,0.));
#11894=DIRECTION('center_axis',(0.,-1.,0.));
#11895=DIRECTION('ref_axis',(1.,0.,0.));
#11896=DIRECTION('center_axis',(0.,1.,0.));
#11897=DIRECTION('ref_axis',(1.,0.,0.));
#11898=DIRECTION('center_axis',(0.,1.,0.));
#11899=DIRECTION('ref_axis',(1.,0.,0.));
#11900=DIRECTION('center_axis',(0.,1.,0.));
#11901=DIRECTION('ref_axis',(1.,0.,0.));
#11902=DIRECTION('center_axis',(0.,1.,0.));
#11903=DIRECTION('ref_axis',(1.,0.,0.));
#11904=DIRECTION('center_axis',(0.,1.,0.));
#11905=DIRECTION('ref_axis',(1.,0.,0.));
#11906=DIRECTION('center_axis',(0.,1.,0.));
#11907=DIRECTION('ref_axis',(1.,0.,0.));
#11908=DIRECTION('center_axis',(0.,-1.,0.));
#11909=DIRECTION('ref_axis',(1.,0.,0.));
#11910=DIRECTION('center_axis',(0.,-1.,0.));
#11911=DIRECTION('ref_axis',(0.,0.,-1.));
#11912=DIRECTION('center_axis',(8.96625347776458E-17,0.,1.));
#11913=DIRECTION('ref_axis',(1.,0.,0.));
#11914=DIRECTION('center_axis',(0.,-1.,0.));
#11915=DIRECTION('ref_axis',(0.,0.,-1.));
#11916=DIRECTION('center_axis',(0.,1.,0.));
#11917=DIRECTION('ref_axis',(1.,0.,0.));
#11918=DIRECTION('center_axis',(0.,-1.,0.));
#11919=DIRECTION('ref_axis',(1.,0.,0.));
#11920=DIRECTION('center_axis',(0.,-1.,0.));
#11921=DIRECTION('ref_axis',(0.,0.,-1.));
#11922=DIRECTION('center_axis',(0.,0.,1.));
#11923=DIRECTION('ref_axis',(1.,0.,0.));
#11924=DIRECTION('center_axis',(0.,-1.,0.));
#11925=DIRECTION('ref_axis',(0.,0.,-1.));
#11926=DIRECTION('center_axis',(0.,1.,0.));
#11927=DIRECTION('ref_axis',(1.,0.,0.));
#11928=DIRECTION('center_axis',(0.,-1.,0.));
#11929=DIRECTION('ref_axis',(1.,0.,0.));
#11930=DIRECTION('center_axis',(0.,-1.,0.));
#11931=DIRECTION('ref_axis',(1.,0.,0.));
#11932=DIRECTION('center_axis',(0.,-1.,0.));
#11933=DIRECTION('ref_axis',(0.,0.,-1.));
#11934=DIRECTION('center_axis',(0.,0.,1.));
#11935=DIRECTION('ref_axis',(1.,0.,0.));
#11936=DIRECTION('center_axis',(0.,-1.,0.));
#11937=DIRECTION('ref_axis',(0.,0.,-1.));
#11938=DIRECTION('center_axis',(0.,1.,0.));
#11939=DIRECTION('ref_axis',(1.,0.,0.));
#11940=DIRECTION('center_axis',(0.,-1.,0.));
#11941=DIRECTION('ref_axis',(1.,0.,0.));
#11942=DIRECTION('center_axis',(0.,-1.,0.));
#11943=DIRECTION('ref_axis',(0.,0.,-1.));
#11944=DIRECTION('center_axis',(8.96625347776458E-17,0.,1.));
#11945=DIRECTION('ref_axis',(1.,0.,0.));
#11946=DIRECTION('center_axis',(0.,-1.,0.));
#11947=DIRECTION('ref_axis',(0.,0.,-1.));
#11948=DIRECTION('center_axis',(0.,1.,0.));
#11949=DIRECTION('ref_axis',(1.,0.,0.));
#11950=DIRECTION('center_axis',(0.,-1.,0.));
#11951=DIRECTION('ref_axis',(1.,0.,0.));
#11952=DIRECTION('center_axis',(0.,-1.,0.));
#11953=DIRECTION('ref_axis',(0.,0.,-1.));
#11954=DIRECTION('center_axis',(0.,0.,1.));
#11955=DIRECTION('ref_axis',(1.,0.,0.));
#11956=DIRECTION('center_axis',(0.,-1.,0.));
#11957=DIRECTION('ref_axis',(0.,0.,-1.));
#11958=DIRECTION('center_axis',(0.,1.,0.));
#11959=DIRECTION('ref_axis',(1.,0.,0.));
#11960=DIRECTION('center_axis',(0.,1.,0.));
#11961=DIRECTION('ref_axis',(1.,0.,0.));
#11962=DIRECTION('',(0.,1.,0.));
#11963=DIRECTION('center_axis',(0.,-1.,0.));
#11964=DIRECTION('ref_axis',(1.,0.,0.));
#11965=DIRECTION('center_axis',(0.,-1.,0.));
#11966=DIRECTION('ref_axis',(1.,0.,0.));
#11967=DIRECTION('center_axis',(0.,1.,0.));
#11968=DIRECTION('ref_axis',(1.,0.,0.));
#11969=DIRECTION('center_axis',(0.,-1.,0.));
#11970=DIRECTION('ref_axis',(0.,0.,-1.));
#11971=DIRECTION('center_axis',(0.,0.,1.));
#11972=DIRECTION('ref_axis',(1.,0.,0.));
#11973=DIRECTION('center_axis',(0.,-1.,0.));
#11974=DIRECTION('ref_axis',(0.,0.,-1.));
#11975=DIRECTION('center_axis',(0.,-1.,0.));
#11976=DIRECTION('ref_axis',(-1.,0.,0.));
#11977=DIRECTION('center_axis',(0.,1.,0.));
#11978=DIRECTION('ref_axis',(1.,0.,0.));
#11979=DIRECTION('axis',(0.,0.,1.));
#11980=DIRECTION('refdir',(1.,0.,0.));
#11981=DIRECTION('center_axis',(0.,1.,0.));
#11982=DIRECTION('ref_axis',(0.,0.,1.));
#11983=DIRECTION('center_axis',(0.,-1.,0.));
#11984=DIRECTION('ref_axis',(1.,0.,0.));
#11985=DIRECTION('center_axis',(0.,-1.,0.));
#11986=DIRECTION('ref_axis',(1.,0.,0.));
#11987=DIRECTION('center_axis',(0.,-1.,0.));
#11988=DIRECTION('ref_axis',(1.,0.,0.));
#11989=DIRECTION('center_axis',(0.,-1.,0.));
#11990=DIRECTION('ref_axis',(1.,0.,0.));
#11991=DIRECTION('',(0.,1.,0.));
#11992=DIRECTION('center_axis',(0.,-1.,0.));
#11993=DIRECTION('ref_axis',(0.,0.,-1.));
#11994=DIRECTION('center_axis',(0.,-1.,0.));
#11995=DIRECTION('ref_axis',(1.,0.,0.));
#11996=DIRECTION('center_axis',(0.,-1.,0.));
#11997=DIRECTION('ref_axis',(1.,0.,0.));
#11998=DIRECTION('',(0.,1.,0.));
#11999=DIRECTION('center_axis',(0.,1.,0.));
#12000=DIRECTION('ref_axis',(0.,0.,1.));
#12001=DIRECTION('center_axis',(0.,-1.,0.));
#12002=DIRECTION('ref_axis',(1.,0.,0.));
#12003=DIRECTION('center_axis',(0.,-1.,0.));
#12004=DIRECTION('ref_axis',(1.,0.,0.));
#12005=DIRECTION('center_axis',(0.,-1.,0.));
#12006=DIRECTION('ref_axis',(1.,0.,0.));
#12007=DIRECTION('center_axis',(0.,-1.,0.));
#12008=DIRECTION('ref_axis',(1.,0.,0.));
#12009=DIRECTION('',(0.,1.,0.));
#12010=DIRECTION('center_axis',(0.,-1.,0.));
#12011=DIRECTION('ref_axis',(0.,0.,-1.));
#12012=DIRECTION('center_axis',(0.,-1.,0.));
#12013=DIRECTION('ref_axis',(1.,0.,0.));
#12014=DIRECTION('center_axis',(0.,-1.,0.));
#12015=DIRECTION('ref_axis',(1.,0.,0.));
#12016=DIRECTION('',(0.,1.,0.));
#12017=DIRECTION('',(0.,0.,1.));
#12018=DIRECTION('',(1.,0.,0.));
#12019=DIRECTION('',(0.,0.,1.));
#12020=DIRECTION('',(1.,0.,0.));
#12021=DIRECTION('',(0.,0.,1.));
#12022=DIRECTION('',(1.,0.,0.));
#12023=DIRECTION('',(0.,0.,1.));
#12024=DIRECTION('',(1.,0.,0.));
#12025=DIRECTION('',(0.,0.,1.));
#12026=DIRECTION('',(1.,0.,0.));
#12027=DIRECTION('axis',(0.,0.,1.));
#12028=DIRECTION('refdir',(1.,0.,0.));
#12029=DIRECTION('axis',(0.,0.,1.));
#12030=DIRECTION('refdir',(1.,0.,0.));
#12031=DIRECTION('center_axis',(1.,0.,0.));
#12032=DIRECTION('ref_axis',(0.,0.,-1.));
#12033=DIRECTION('center_axis',(1.,0.,0.));
#12034=DIRECTION('ref_axis',(0.,0.,-1.));
#12035=DIRECTION('',(1.,0.,0.));
#12036=DIRECTION('center_axis',(-1.,0.,0.));
#12037=DIRECTION('ref_axis',(0.,0.,-1.));
#12038=DIRECTION('center_axis',(1.,0.,0.));
#12039=DIRECTION('ref_axis',(0.,0.,-1.));
#12040=DIRECTION('center_axis',(1.,0.,0.));
#12041=DIRECTION('ref_axis',(0.,0.,-1.));
#12042=DIRECTION('center_axis',(1.,0.,0.));
#12043=DIRECTION('ref_axis',(0.,0.,-1.));
#12044=DIRECTION('',(1.,0.,0.));
#12045=DIRECTION('center_axis',(-1.,0.,0.));
#12046=DIRECTION('ref_axis',(0.,0.,-1.));
#12047=DIRECTION('center_axis',(1.,0.,0.));
#12048=DIRECTION('ref_axis',(0.,0.,-1.));
#12049=DIRECTION('center_axis',(1.,0.,0.));
#12050=DIRECTION('ref_axis',(0.,0.,-1.));
#12051=DIRECTION('center_axis',(1.,0.,0.));
#12052=DIRECTION('ref_axis',(0.,0.,-1.));
#12053=DIRECTION('',(1.,0.,0.));
#12054=DIRECTION('center_axis',(-1.,0.,0.));
#12055=DIRECTION('ref_axis',(0.,0.,-1.));
#12056=DIRECTION('center_axis',(1.,0.,0.));
#12057=DIRECTION('ref_axis',(0.,0.,-1.));
#12058=DIRECTION('center_axis',(1.,0.,0.));
#12059=DIRECTION('ref_axis',(0.,0.,-1.));
#12060=DIRECTION('center_axis',(1.,0.,0.));
#12061=DIRECTION('ref_axis',(0.,0.,-1.));
#12062=DIRECTION('',(1.,0.,0.));
#12063=DIRECTION('center_axis',(-1.,0.,0.));
#12064=DIRECTION('ref_axis',(0.,0.,-1.));
#12065=DIRECTION('center_axis',(1.,0.,0.));
#12066=DIRECTION('ref_axis',(0.,0.,-1.));
#12067=DIRECTION('center_axis',(1.,0.,0.));
#12068=DIRECTION('ref_axis',(0.,0.,-1.));
#12069=DIRECTION('center_axis',(1.,0.,0.));
#12070=DIRECTION('ref_axis',(0.,0.,-1.));
#12071=DIRECTION('',(1.,0.,0.));
#12072=DIRECTION('center_axis',(-1.,0.,0.));
#12073=DIRECTION('ref_axis',(0.,0.,-1.));
#12074=DIRECTION('center_axis',(1.,0.,0.));
#12075=DIRECTION('ref_axis',(0.,0.,-1.));
#12076=DIRECTION('center_axis',(1.,0.,0.));
#12077=DIRECTION('ref_axis',(0.,0.,-1.));
#12078=DIRECTION('center_axis',(1.,0.,0.));
#12079=DIRECTION('ref_axis',(0.,0.,-1.));
#12080=DIRECTION('',(1.,0.,0.));
#12081=DIRECTION('center_axis',(-1.,0.,0.));
#12082=DIRECTION('ref_axis',(0.,0.,-1.));
#12083=DIRECTION('center_axis',(1.,0.,0.));
#12084=DIRECTION('ref_axis',(0.,0.,-1.));
#12085=DIRECTION('center_axis',(1.,0.,0.));
#12086=DIRECTION('ref_axis',(0.,0.,-1.));
#12087=DIRECTION('center_axis',(1.,0.,0.));
#12088=DIRECTION('ref_axis',(0.,0.,-1.));
#12089=DIRECTION('',(1.,0.,0.));
#12090=DIRECTION('center_axis',(-1.,0.,0.));
#12091=DIRECTION('ref_axis',(0.,0.,-1.));
#12092=DIRECTION('center_axis',(1.,0.,0.));
#12093=DIRECTION('ref_axis',(0.,0.,-1.));
#12094=DIRECTION('center_axis',(1.,0.,0.));
#12095=DIRECTION('ref_axis',(0.,0.,-1.));
#12096=DIRECTION('',(1.,0.,0.));
#12097=DIRECTION('center_axis',(-1.,0.,0.));
#12098=DIRECTION('ref_axis',(0.,0.,-1.));
#12099=DIRECTION('center_axis',(1.,0.,0.));
#12100=DIRECTION('ref_axis',(0.,0.,-1.));
#12101=DIRECTION('center_axis',(1.,0.,0.));
#12102=DIRECTION('ref_axis',(0.,0.,-1.));
#12103=DIRECTION('',(1.,0.,0.));
#12104=DIRECTION('center_axis',(-1.,0.,0.));
#12105=DIRECTION('ref_axis',(0.,0.,-1.));
#12106=DIRECTION('center_axis',(1.,0.,0.));
#12107=DIRECTION('ref_axis',(0.,0.,-1.));
#12108=DIRECTION('center_axis',(1.,0.,0.));
#12109=DIRECTION('ref_axis',(0.,0.,-1.));
#12110=DIRECTION('',(1.,0.,0.));
#12111=DIRECTION('center_axis',(-1.,0.,0.));
#12112=DIRECTION('ref_axis',(0.,0.,-1.));
#12113=DIRECTION('center_axis',(1.,0.,0.));
#12114=DIRECTION('ref_axis',(0.,0.,-1.));
#12115=DIRECTION('center_axis',(1.,0.,0.));
#12116=DIRECTION('ref_axis',(0.,0.,-1.));
#12117=DIRECTION('',(1.,0.,0.));
#12118=DIRECTION('center_axis',(-1.,0.,0.));
#12119=DIRECTION('ref_axis',(0.,0.,-1.));
#12120=DIRECTION('center_axis',(1.,0.,0.));
#12121=DIRECTION('ref_axis',(0.,0.,-1.));
#12122=DIRECTION('center_axis',(1.,0.,0.));
#12123=DIRECTION('ref_axis',(0.,0.,-1.));
#12124=DIRECTION('',(1.,0.,0.));
#12125=DIRECTION('center_axis',(-1.,0.,0.));
#12126=DIRECTION('ref_axis',(0.,0.,-1.));
#12127=DIRECTION('center_axis',(1.,0.,0.));
#12128=DIRECTION('ref_axis',(0.,0.,-1.));
#12129=DIRECTION('center_axis',(1.,0.,0.));
#12130=DIRECTION('ref_axis',(0.,0.,-1.));
#12131=DIRECTION('',(1.,0.,0.));
#12132=DIRECTION('center_axis',(-1.,0.,0.));
#12133=DIRECTION('ref_axis',(0.,0.,-1.));
#12134=DIRECTION('center_axis',(0.,1.,0.));
#12135=DIRECTION('ref_axis',(-1.,0.,0.));
#12136=DIRECTION('',(-1.,0.,0.));
#12137=DIRECTION('',(0.,0.,1.));
#12138=DIRECTION('',(-1.,0.,0.));
#12139=DIRECTION('',(0.,0.,1.));
#12140=DIRECTION('center_axis',(1.,0.,0.));
#12141=DIRECTION('ref_axis',(0.,1.,0.));
#12142=DIRECTION('',(0.,1.,0.));
#12143=DIRECTION('',(0.,1.,0.));
#12144=DIRECTION('',(0.,0.,1.));
#12145=DIRECTION('center_axis',(0.,-1.,0.));
#12146=DIRECTION('ref_axis',(1.,0.,0.));
#12147=DIRECTION('',(1.,0.,0.));
#12148=DIRECTION('',(1.,0.,0.));
#12149=DIRECTION('',(0.,0.,1.));
#12150=DIRECTION('center_axis',(-1.,0.,0.));
#12151=DIRECTION('ref_axis',(0.,-1.,0.));
#12152=DIRECTION('',(0.,-1.,0.));
#12153=DIRECTION('',(0.,-1.,0.));
#12154=DIRECTION('center_axis',(0.,0.,1.));
#12155=DIRECTION('ref_axis',(1.,0.,0.));
#12156=DIRECTION('center_axis',(0.,0.,1.));
#12157=DIRECTION('ref_axis',(1.,0.,0.));
#12158=DIRECTION('axis',(0.,0.,1.));
#12159=DIRECTION('refdir',(1.,0.,0.));
#12160=DIRECTION('center_axis',(1.,0.,0.));
#12161=DIRECTION('ref_axis',(0.,0.,-1.));
#12162=DIRECTION('center_axis',(1.,0.,0.));
#12163=DIRECTION('ref_axis',(0.,0.,-1.));
#12164=DIRECTION('',(1.,0.,0.));
#12165=DIRECTION('center_axis',(-1.,0.,0.));
#12166=DIRECTION('ref_axis',(0.,0.,-1.));
#12167=DIRECTION('center_axis',(1.,0.,0.));
#12168=DIRECTION('ref_axis',(0.,0.,-1.));
#12169=DIRECTION('center_axis',(1.,0.,0.));
#12170=DIRECTION('ref_axis',(0.,0.,-1.));
#12171=DIRECTION('',(1.,0.,0.));
#12172=DIRECTION('center_axis',(-1.,0.,0.));
#12173=DIRECTION('ref_axis',(0.,0.,-1.));
#12174=DIRECTION('center_axis',(1.,0.,0.));
#12175=DIRECTION('ref_axis',(0.,0.,-1.));
#12176=DIRECTION('center_axis',(1.,0.,0.));
#12177=DIRECTION('ref_axis',(0.,0.,-1.));
#12178=DIRECTION('',(1.,0.,0.));
#12179=DIRECTION('center_axis',(-1.,0.,0.));
#12180=DIRECTION('ref_axis',(0.,0.,-1.));
#12181=DIRECTION('center_axis',(1.,0.,0.));
#12182=DIRECTION('ref_axis',(0.,0.,-1.));
#12183=DIRECTION('center_axis',(1.,0.,0.));
#12184=DIRECTION('ref_axis',(0.,0.,-1.));
#12185=DIRECTION('',(1.,0.,0.));
#12186=DIRECTION('center_axis',(-1.,0.,0.));
#12187=DIRECTION('ref_axis',(0.,0.,-1.));
#12188=DIRECTION('center_axis',(1.,0.,0.));
#12189=DIRECTION('ref_axis',(0.,0.,-1.));
#12190=DIRECTION('center_axis',(1.,0.,0.));
#12191=DIRECTION('ref_axis',(0.,0.,-1.));
#12192=DIRECTION('',(1.,0.,0.));
#12193=DIRECTION('center_axis',(-1.,0.,0.));
#12194=DIRECTION('ref_axis',(0.,0.,-1.));
#12195=DIRECTION('center_axis',(1.,0.,0.));
#12196=DIRECTION('ref_axis',(0.,0.,-1.));
#12197=DIRECTION('center_axis',(1.,0.,0.));
#12198=DIRECTION('ref_axis',(0.,0.,-1.));
#12199=DIRECTION('',(1.,0.,0.));
#12200=DIRECTION('center_axis',(-1.,0.,0.));
#12201=DIRECTION('ref_axis',(0.,0.,-1.));
#12202=DIRECTION('center_axis',(1.,0.,0.));
#12203=DIRECTION('ref_axis',(0.,0.,-1.));
#12204=DIRECTION('center_axis',(1.,0.,0.));
#12205=DIRECTION('ref_axis',(0.,0.,-1.));
#12206=DIRECTION('',(1.,0.,0.));
#12207=DIRECTION('center_axis',(-1.,0.,0.));
#12208=DIRECTION('ref_axis',(0.,0.,-1.));
#12209=DIRECTION('center_axis',(0.,1.,0.));
#12210=DIRECTION('ref_axis',(-1.,0.,0.));
#12211=DIRECTION('',(-1.,0.,0.));
#12212=DIRECTION('',(0.,0.,1.));
#12213=DIRECTION('',(-1.,0.,0.));
#12214=DIRECTION('',(0.,0.,1.));
#12215=DIRECTION('center_axis',(1.,0.,0.));
#12216=DIRECTION('ref_axis',(0.,1.,0.));
#12217=DIRECTION('',(0.,1.,0.));
#12218=DIRECTION('',(0.,1.,0.));
#12219=DIRECTION('',(0.,0.,1.));
#12220=DIRECTION('center_axis',(0.,-1.,0.));
#12221=DIRECTION('ref_axis',(1.,0.,0.));
#12222=DIRECTION('',(1.,0.,0.));
#12223=DIRECTION('',(1.,0.,0.));
#12224=DIRECTION('',(0.,0.,1.));
#12225=DIRECTION('center_axis',(-1.,0.,0.));
#12226=DIRECTION('ref_axis',(0.,-1.,0.));
#12227=DIRECTION('',(0.,-1.,0.));
#12228=DIRECTION('',(0.,-1.,0.));
#12229=DIRECTION('center_axis',(0.,0.,1.));
#12230=DIRECTION('ref_axis',(1.,0.,0.));
#12231=DIRECTION('center_axis',(0.,0.,1.));
#12232=DIRECTION('ref_axis',(1.,0.,0.));
#12233=DIRECTION('axis',(0.,0.,1.));
#12234=DIRECTION('refdir',(1.,0.,0.));
#12235=DIRECTION('center_axis',(1.,0.,0.));
#12236=DIRECTION('ref_axis',(0.,0.,-1.));
#12237=DIRECTION('center_axis',(1.,0.,0.));
#12238=DIRECTION('ref_axis',(0.,0.,-1.));
#12239=DIRECTION('',(1.,0.,0.));
#12240=DIRECTION('center_axis',(-1.,0.,0.));
#12241=DIRECTION('ref_axis',(0.,0.,-1.));
#12242=DIRECTION('center_axis',(1.,0.,0.));
#12243=DIRECTION('ref_axis',(0.,0.,-1.));
#12244=DIRECTION('center_axis',(1.,0.,0.));
#12245=DIRECTION('ref_axis',(0.,0.,-1.));
#12246=DIRECTION('',(1.,0.,0.));
#12247=DIRECTION('center_axis',(-1.,0.,0.));
#12248=DIRECTION('ref_axis',(0.,0.,-1.));
#12249=DIRECTION('center_axis',(1.,0.,0.));
#12250=DIRECTION('ref_axis',(0.,0.,-1.));
#12251=DIRECTION('center_axis',(1.,0.,0.));
#12252=DIRECTION('ref_axis',(0.,0.,-1.));
#12253=DIRECTION('',(1.,0.,0.));
#12254=DIRECTION('center_axis',(-1.,0.,0.));
#12255=DIRECTION('ref_axis',(0.,0.,-1.));
#12256=DIRECTION('center_axis',(1.,0.,0.));
#12257=DIRECTION('ref_axis',(0.,0.,-1.));
#12258=DIRECTION('center_axis',(1.,0.,0.));
#12259=DIRECTION('ref_axis',(0.,0.,-1.));
#12260=DIRECTION('',(1.,0.,0.));
#12261=DIRECTION('center_axis',(-1.,0.,0.));
#12262=DIRECTION('ref_axis',(0.,0.,-1.));
#12263=DIRECTION('center_axis',(1.,0.,0.));
#12264=DIRECTION('ref_axis',(0.,0.,-1.));
#12265=DIRECTION('center_axis',(1.,0.,0.));
#12266=DIRECTION('ref_axis',(0.,0.,-1.));
#12267=DIRECTION('',(1.,0.,0.));
#12268=DIRECTION('center_axis',(-1.,0.,0.));
#12269=DIRECTION('ref_axis',(0.,0.,-1.));
#12270=DIRECTION('center_axis',(1.,0.,0.));
#12271=DIRECTION('ref_axis',(0.,0.,-1.));
#12272=DIRECTION('center_axis',(1.,0.,0.));
#12273=DIRECTION('ref_axis',(0.,0.,-1.));
#12274=DIRECTION('',(1.,0.,0.));
#12275=DIRECTION('center_axis',(-1.,0.,0.));
#12276=DIRECTION('ref_axis',(0.,0.,-1.));
#12277=DIRECTION('center_axis',(1.,0.,0.));
#12278=DIRECTION('ref_axis',(0.,0.,-1.));
#12279=DIRECTION('center_axis',(1.,0.,0.));
#12280=DIRECTION('ref_axis',(0.,0.,-1.));
#12281=DIRECTION('',(1.,0.,0.));
#12282=DIRECTION('center_axis',(-1.,0.,0.));
#12283=DIRECTION('ref_axis',(0.,0.,-1.));
#12284=DIRECTION('center_axis',(0.,1.,0.));
#12285=DIRECTION('ref_axis',(-1.,0.,0.));
#12286=DIRECTION('',(-1.,0.,0.));
#12287=DIRECTION('',(0.,0.,1.));
#12288=DIRECTION('',(-1.,0.,0.));
#12289=DIRECTION('',(0.,0.,1.));
#12290=DIRECTION('center_axis',(1.,0.,0.));
#12291=DIRECTION('ref_axis',(0.,1.,0.));
#12292=DIRECTION('',(0.,1.,0.));
#12293=DIRECTION('',(0.,1.,0.));
#12294=DIRECTION('',(0.,0.,1.));
#12295=DIRECTION('center_axis',(0.,-1.,0.));
#12296=DIRECTION('ref_axis',(1.,0.,0.));
#12297=DIRECTION('',(1.,0.,0.));
#12298=DIRECTION('',(1.,0.,0.));
#12299=DIRECTION('',(0.,0.,1.));
#12300=DIRECTION('center_axis',(-1.,0.,0.));
#12301=DIRECTION('ref_axis',(0.,-1.,0.));
#12302=DIRECTION('',(0.,-1.,0.));
#12303=DIRECTION('',(0.,-1.,0.));
#12304=DIRECTION('center_axis',(0.,0.,1.));
#12305=DIRECTION('ref_axis',(1.,0.,0.));
#12306=DIRECTION('center_axis',(0.,0.,1.));
#12307=DIRECTION('ref_axis',(1.,0.,0.));
#12308=DIRECTION('axis',(0.,0.,1.));
#12309=DIRECTION('refdir',(1.,0.,0.));
#12310=DIRECTION('center_axis',(1.,0.,0.));
#12311=DIRECTION('ref_axis',(0.,0.,-1.));
#12312=DIRECTION('center_axis',(-1.,0.,0.));
#12313=DIRECTION('ref_axis',(0.,0.,-1.));
#12314=DIRECTION('center_axis',(1.,0.,0.));
#12315=DIRECTION('ref_axis',(0.,0.,-1.));
#12316=DIRECTION('center_axis',(1.,0.,0.));
#12317=DIRECTION('ref_axis',(0.,0.,-1.));
#12318=DIRECTION('center_axis',(1.,0.,0.));
#12319=DIRECTION('ref_axis',(0.,0.,-1.));
#12320=DIRECTION('',(-1.,0.,0.));
#12321=DIRECTION('center_axis',(1.,0.,0.));
#12322=DIRECTION('ref_axis',(0.,0.,-1.));
#12323=DIRECTION('',(1.,0.,0.));
#12324=DIRECTION('',(1.,0.,0.));
#12325=DIRECTION('center_axis',(-1.,0.,0.));
#12326=DIRECTION('ref_axis',(0.,0.,-1.));
#12327=DIRECTION('center_axis',(1.,0.,0.));
#12328=DIRECTION('ref_axis',(0.,0.,-1.));
#12329=DIRECTION('center_axis',(-1.,0.,0.));
#12330=DIRECTION('ref_axis',(0.,0.,-1.));
#12331=DIRECTION('center_axis',(1.,0.,0.));
#12332=DIRECTION('ref_axis',(0.,0.,-1.));
#12333=DIRECTION('center_axis',(-1.,0.,0.));
#12334=DIRECTION('ref_axis',(0.,0.,-1.));
#12335=DIRECTION('center_axis',(1.,0.,0.));
#12336=DIRECTION('ref_axis',(0.,0.,-1.));
#12337=DIRECTION('',(-1.,0.,0.));
#12338=DIRECTION('center_axis',(1.,0.,0.));
#12339=DIRECTION('ref_axis',(0.,0.,-1.));
#12340=DIRECTION('',(1.,0.,0.));
#12341=DIRECTION('center_axis',(-1.,0.,0.));
#12342=DIRECTION('ref_axis',(0.,0.,-1.));
#12343=DIRECTION('center_axis',(1.,0.,0.));
#12344=DIRECTION('ref_axis',(0.,0.,-1.));
#12345=DIRECTION('',(1.,0.,0.));
#12346=DIRECTION('center_axis',(1.,0.,0.));
#12347=DIRECTION('ref_axis',(0.,0.,-1.));
#12348=DIRECTION('center_axis',(1.,0.,0.));
#12349=DIRECTION('ref_axis',(0.,0.,-1.));
#12350=DIRECTION('',(-1.,0.,0.));
#12351=DIRECTION('center_axis',(1.,0.,0.));
#12352=DIRECTION('ref_axis',(0.,0.,-1.));
#12353=DIRECTION('center_axis',(1.,0.,0.));
#12354=DIRECTION('ref_axis',(0.,0.,-1.));
#12355=DIRECTION('center_axis',(1.,0.,0.));
#12356=DIRECTION('ref_axis',(0.,0.,-1.));
#12357=DIRECTION('center_axis',(1.,0.,0.));
#12358=DIRECTION('ref_axis',(0.,0.,-1.));
#12359=DIRECTION('center_axis',(1.,0.,0.));
#12360=DIRECTION('ref_axis',(0.,0.,-1.));
#12361=DIRECTION('center_axis',(1.,0.,0.));
#12362=DIRECTION('ref_axis',(0.,0.,-1.));
#12363=DIRECTION('',(-1.,0.,0.));
#12364=DIRECTION('center_axis',(1.,0.,0.));
#12365=DIRECTION('ref_axis',(0.,0.,-1.));
#12366=DIRECTION('center_axis',(-1.,0.,0.));
#12367=DIRECTION('ref_axis',(0.,0.,-1.));
#12368=DIRECTION('center_axis',(1.,0.,0.));
#12369=DIRECTION('ref_axis',(0.,0.,-1.));
#12370=DIRECTION('',(-1.,0.,0.));
#12371=DIRECTION('center_axis',(-1.,0.,0.));
#12372=DIRECTION('ref_axis',(0.,0.,-1.));
#12373=DIRECTION('center_axis',(1.,0.,0.));
#12374=DIRECTION('ref_axis',(0.,0.,-1.));
#12375=DIRECTION('axis',(0.,0.,1.));
#12376=DIRECTION('refdir',(1.,0.,0.));
#12377=DIRECTION('center_axis',(1.,0.,0.));
#12378=DIRECTION('ref_axis',(0.,0.,-1.));
#12379=DIRECTION('center_axis',(1.,0.,0.));
#12380=DIRECTION('ref_axis',(0.,0.,-1.));
#12381=DIRECTION('',(1.,0.,0.));
#12382=DIRECTION('center_axis',(-1.,0.,0.));
#12383=DIRECTION('ref_axis',(0.,0.,-1.));
#12384=DIRECTION('center_axis',(1.,0.,0.));
#12385=DIRECTION('ref_axis',(0.,0.,-1.));
#12386=DIRECTION('center_axis',(1.,0.,0.));
#12387=DIRECTION('ref_axis',(0.,0.,-1.));
#12388=DIRECTION('center_axis',(1.,0.,0.));
#12389=DIRECTION('ref_axis',(0.,0.,-1.));
#12390=DIRECTION('center_axis',(1.,0.,0.));
#12391=DIRECTION('ref_axis',(0.,0.,-1.));
#12392=DIRECTION('',(1.,0.,0.));
#12393=DIRECTION('center_axis',(-1.,0.,0.));
#12394=DIRECTION('ref_axis',(0.,0.,-1.));
#12395=DIRECTION('center_axis',(1.,0.,0.));
#12396=DIRECTION('ref_axis',(0.,0.,-1.));
#12397=DIRECTION('center_axis',(1.,0.,0.));
#12398=DIRECTION('ref_axis',(0.,0.,-1.));
#12399=DIRECTION('center_axis',(1.,0.,0.));
#12400=DIRECTION('ref_axis',(0.,0.,-1.));
#12401=DIRECTION('center_axis',(1.,0.,0.));
#12402=DIRECTION('ref_axis',(0.,0.,-1.));
#12403=DIRECTION('',(1.,0.,0.));
#12404=DIRECTION('center_axis',(-1.,0.,0.));
#12405=DIRECTION('ref_axis',(0.,0.,-1.));
#12406=DIRECTION('center_axis',(1.,0.,0.));
#12407=DIRECTION('ref_axis',(0.,0.,-1.));
#12408=DIRECTION('center_axis',(1.,0.,0.));
#12409=DIRECTION('ref_axis',(0.,0.,-1.));
#12410=DIRECTION('center_axis',(1.,0.,0.));
#12411=DIRECTION('ref_axis',(0.,0.,-1.));
#12412=DIRECTION('center_axis',(1.,0.,0.));
#12413=DIRECTION('ref_axis',(0.,0.,-1.));
#12414=DIRECTION('',(1.,0.,0.));
#12415=DIRECTION('center_axis',(-1.,0.,0.));
#12416=DIRECTION('ref_axis',(0.,0.,-1.));
#12417=DIRECTION('center_axis',(1.,0.,0.));
#12418=DIRECTION('ref_axis',(0.,0.,-1.));
#12419=DIRECTION('center_axis',(1.,0.,0.));
#12420=DIRECTION('ref_axis',(0.,0.,-1.));
#12421=DIRECTION('center_axis',(1.,0.,0.));
#12422=DIRECTION('ref_axis',(0.,0.,-1.));
#12423=DIRECTION('center_axis',(1.,0.,0.));
#12424=DIRECTION('ref_axis',(0.,0.,-1.));
#12425=DIRECTION('',(1.,0.,0.));
#12426=DIRECTION('center_axis',(1.,0.,0.));
#12427=DIRECTION('ref_axis',(0.,0.,-1.));
#12428=DIRECTION('center_axis',(1.,0.,0.));
#12429=DIRECTION('ref_axis',(0.,0.,-1.));
#12430=DIRECTION('',(1.,0.,0.));
#12431=DIRECTION('center_axis',(1.,0.,0.));
#12432=DIRECTION('ref_axis',(0.,0.,-1.));
#12433=DIRECTION('center_axis',(1.,0.,0.));
#12434=DIRECTION('ref_axis',(0.,0.,-1.));
#12435=DIRECTION('',(1.,0.,0.));
#12436=DIRECTION('center_axis',(1.,0.,0.));
#12437=DIRECTION('ref_axis',(0.,0.,-1.));
#12438=DIRECTION('center_axis',(1.,0.,0.));
#12439=DIRECTION('ref_axis',(0.,0.,-1.));
#12440=DIRECTION('',(1.,0.,0.));
#12441=DIRECTION('center_axis',(0.,1.,0.));
#12442=DIRECTION('ref_axis',(-1.,0.,0.));
#12443=DIRECTION('',(-1.,0.,0.));
#12444=DIRECTION('',(0.,0.,1.));
#12445=DIRECTION('',(-1.,0.,0.));
#12446=DIRECTION('',(0.,0.,1.));
#12447=DIRECTION('center_axis',(1.,0.,0.));
#12448=DIRECTION('ref_axis',(0.,1.,0.));
#12449=DIRECTION('',(0.,1.,0.));
#12450=DIRECTION('',(0.,1.,0.));
#12451=DIRECTION('',(0.,0.,1.));
#12452=DIRECTION('center_axis',(0.,-1.,0.));
#12453=DIRECTION('ref_axis',(1.,0.,0.));
#12454=DIRECTION('',(1.,0.,0.));
#12455=DIRECTION('',(1.,0.,0.));
#12456=DIRECTION('',(0.,0.,1.));
#12457=DIRECTION('center_axis',(-1.,0.,0.));
#12458=DIRECTION('ref_axis',(0.,-1.,0.));
#12459=DIRECTION('',(0.,-1.,0.));
#12460=DIRECTION('',(0.,-1.,0.));
#12461=DIRECTION('center_axis',(0.,0.,1.));
#12462=DIRECTION('ref_axis',(1.,0.,0.));
#12463=DIRECTION('center_axis',(0.,0.,1.));
#12464=DIRECTION('ref_axis',(1.,0.,0.));
#12465=DIRECTION('axis',(0.,0.,1.));
#12466=DIRECTION('refdir',(1.,0.,0.));
#12467=DIRECTION('axis',(0.,0.,1.));
#12468=DIRECTION('refdir',(1.,0.,0.));
#12469=DIRECTION('center_axis',(1.,0.,0.));
#12470=DIRECTION('ref_axis',(0.,0.,-1.));
#12471=DIRECTION('center_axis',(1.,0.,0.));
#12472=DIRECTION('ref_axis',(0.,0.,-1.));
#12473=DIRECTION('',(1.,0.,0.));
#12474=DIRECTION('center_axis',(1.,0.,0.));
#12475=DIRECTION('ref_axis',(0.,0.,-1.));
#12476=DIRECTION('center_axis',(1.,0.,0.));
#12477=DIRECTION('ref_axis',(0.,0.,-1.));
#12478=DIRECTION('center_axis',(1.,0.,0.));
#12479=DIRECTION('ref_axis',(0.,0.,-1.));
#12480=DIRECTION('center_axis',(1.,0.,0.));
#12481=DIRECTION('ref_axis',(0.,0.,-1.));
#12482=DIRECTION('',(1.,0.,0.));
#12483=DIRECTION('center_axis',(1.,0.,0.));
#12484=DIRECTION('ref_axis',(0.,0.,-1.));
#12485=DIRECTION('center_axis',(1.,0.,0.));
#12486=DIRECTION('ref_axis',(0.,0.,-1.));
#12487=DIRECTION('center_axis',(1.,0.,0.));
#12488=DIRECTION('ref_axis',(0.,0.,-1.));
#12489=DIRECTION('center_axis',(1.,0.,0.));
#12490=DIRECTION('ref_axis',(0.,0.,-1.));
#12491=DIRECTION('',(1.,0.,0.));
#12492=DIRECTION('center_axis',(1.,0.,0.));
#12493=DIRECTION('ref_axis',(0.,0.,-1.));
#12494=DIRECTION('center_axis',(1.,0.,0.));
#12495=DIRECTION('ref_axis',(0.,0.,-1.));
#12496=DIRECTION('center_axis',(1.,0.,0.));
#12497=DIRECTION('ref_axis',(0.,0.,-1.));
#12498=DIRECTION('center_axis',(1.,0.,0.));
#12499=DIRECTION('ref_axis',(0.,0.,-1.));
#12500=DIRECTION('',(1.,0.,0.));
#12501=DIRECTION('center_axis',(1.,0.,0.));
#12502=DIRECTION('ref_axis',(0.,0.,-1.));
#12503=DIRECTION('center_axis',(1.,0.,0.));
#12504=DIRECTION('ref_axis',(0.,0.,-1.));
#12505=DIRECTION('center_axis',(1.,0.,0.));
#12506=DIRECTION('ref_axis',(0.,0.,-1.));
#12507=DIRECTION('center_axis',(1.,0.,0.));
#12508=DIRECTION('ref_axis',(0.,0.,-1.));
#12509=DIRECTION('',(1.,0.,0.));
#12510=DIRECTION('center_axis',(1.,0.,0.));
#12511=DIRECTION('ref_axis',(0.,0.,-1.));
#12512=DIRECTION('center_axis',(1.,0.,0.));
#12513=DIRECTION('ref_axis',(0.,0.,-1.));
#12514=DIRECTION('center_axis',(1.,0.,0.));
#12515=DIRECTION('ref_axis',(0.,0.,-1.));
#12516=DIRECTION('center_axis',(1.,0.,0.));
#12517=DIRECTION('ref_axis',(0.,0.,-1.));
#12518=DIRECTION('',(1.,0.,0.));
#12519=DIRECTION('center_axis',(1.,0.,0.));
#12520=DIRECTION('ref_axis',(0.,0.,-1.));
#12521=DIRECTION('center_axis',(1.,0.,0.));
#12522=DIRECTION('ref_axis',(0.,0.,-1.));
#12523=DIRECTION('center_axis',(1.,0.,0.));
#12524=DIRECTION('ref_axis',(0.,0.,-1.));
#12525=DIRECTION('center_axis',(1.,0.,0.));
#12526=DIRECTION('ref_axis',(0.,0.,-1.));
#12527=DIRECTION('',(1.,0.,0.));
#12528=DIRECTION('center_axis',(-1.,0.,0.));
#12529=DIRECTION('ref_axis',(0.,0.,-1.));
#12530=DIRECTION('center_axis',(1.,0.,0.));
#12531=DIRECTION('ref_axis',(0.,0.,-1.));
#12532=DIRECTION('center_axis',(1.,0.,0.));
#12533=DIRECTION('ref_axis',(0.,0.,-1.));
#12534=DIRECTION('',(1.,0.,0.));
#12535=DIRECTION('center_axis',(-1.,0.,0.));
#12536=DIRECTION('ref_axis',(0.,0.,-1.));
#12537=DIRECTION('center_axis',(1.,0.,0.));
#12538=DIRECTION('ref_axis',(0.,0.,-1.));
#12539=DIRECTION('center_axis',(1.,0.,0.));
#12540=DIRECTION('ref_axis',(0.,0.,-1.));
#12541=DIRECTION('',(1.,0.,0.));
#12542=DIRECTION('center_axis',(-1.,0.,0.));
#12543=DIRECTION('ref_axis',(0.,0.,-1.));
#12544=DIRECTION('center_axis',(1.,0.,0.));
#12545=DIRECTION('ref_axis',(0.,0.,-1.));
#12546=DIRECTION('center_axis',(1.,0.,0.));
#12547=DIRECTION('ref_axis',(0.,0.,-1.));
#12548=DIRECTION('',(1.,0.,0.));
#12549=DIRECTION('center_axis',(-1.,0.,0.));
#12550=DIRECTION('ref_axis',(0.,0.,-1.));
#12551=DIRECTION('center_axis',(1.,0.,0.));
#12552=DIRECTION('ref_axis',(0.,0.,-1.));
#12553=DIRECTION('center_axis',(1.,0.,0.));
#12554=DIRECTION('ref_axis',(0.,0.,-1.));
#12555=DIRECTION('',(1.,0.,0.));
#12556=DIRECTION('center_axis',(-1.,0.,0.));
#12557=DIRECTION('ref_axis',(0.,0.,-1.));
#12558=DIRECTION('center_axis',(1.,0.,0.));
#12559=DIRECTION('ref_axis',(0.,0.,-1.));
#12560=DIRECTION('center_axis',(1.,0.,0.));
#12561=DIRECTION('ref_axis',(0.,0.,-1.));
#12562=DIRECTION('',(1.,0.,0.));
#12563=DIRECTION('center_axis',(-1.,0.,0.));
#12564=DIRECTION('ref_axis',(0.,0.,-1.));
#12565=DIRECTION('center_axis',(1.,0.,0.));
#12566=DIRECTION('ref_axis',(0.,0.,-1.));
#12567=DIRECTION('center_axis',(1.,0.,0.));
#12568=DIRECTION('ref_axis',(0.,0.,-1.));
#12569=DIRECTION('',(1.,0.,0.));
#12570=DIRECTION('center_axis',(-1.,0.,0.));
#12571=DIRECTION('ref_axis',(0.,0.,-1.));
#12572=DIRECTION('center_axis',(0.,1.,0.));
#12573=DIRECTION('ref_axis',(-1.,0.,0.));
#12574=DIRECTION('',(-1.,0.,0.));
#12575=DIRECTION('',(0.,0.,1.));
#12576=DIRECTION('',(-1.,0.,0.));
#12577=DIRECTION('',(0.,0.,1.));
#12578=DIRECTION('center_axis',(1.,0.,0.));
#12579=DIRECTION('ref_axis',(0.,1.,0.));
#12580=DIRECTION('',(0.,1.,0.));
#12581=DIRECTION('',(0.,1.,0.));
#12582=DIRECTION('',(0.,0.,1.));
#12583=DIRECTION('center_axis',(0.,-1.,0.));
#12584=DIRECTION('ref_axis',(1.,0.,0.));
#12585=DIRECTION('',(1.,0.,0.));
#12586=DIRECTION('',(1.,0.,0.));
#12587=DIRECTION('',(0.,0.,1.));
#12588=DIRECTION('center_axis',(-1.,0.,0.));
#12589=DIRECTION('ref_axis',(0.,-1.,0.));
#12590=DIRECTION('',(0.,-1.,0.));
#12591=DIRECTION('',(0.,-1.,0.));
#12592=DIRECTION('center_axis',(0.,0.,1.));
#12593=DIRECTION('ref_axis',(1.,0.,0.));
#12594=DIRECTION('center_axis',(0.,0.,1.));
#12595=DIRECTION('ref_axis',(1.,0.,0.));
#12596=DIRECTION('axis',(0.,0.,1.));
#12597=DIRECTION('refdir',(1.,0.,0.));
#12598=DIRECTION('center_axis',(1.,0.,0.));
#12599=DIRECTION('ref_axis',(0.,0.,-1.));
#12600=DIRECTION('center_axis',(1.,0.,0.));
#12601=DIRECTION('ref_axis',(0.,0.,-1.));
#12602=DIRECTION('',(1.,0.,0.));
#12603=DIRECTION('center_axis',(-1.,0.,0.));
#12604=DIRECTION('ref_axis',(0.,0.,-1.));
#12605=DIRECTION('center_axis',(1.,0.,0.));
#12606=DIRECTION('ref_axis',(0.,0.,-1.));
#12607=DIRECTION('center_axis',(1.,0.,0.));
#12608=DIRECTION('ref_axis',(0.,0.,-1.));
#12609=DIRECTION('',(1.,0.,0.));
#12610=DIRECTION('center_axis',(-1.,0.,0.));
#12611=DIRECTION('ref_axis',(0.,0.,-1.));
#12612=DIRECTION('center_axis',(1.,0.,0.));
#12613=DIRECTION('ref_axis',(0.,0.,-1.));
#12614=DIRECTION('center_axis',(1.,0.,0.));
#12615=DIRECTION('ref_axis',(0.,0.,-1.));
#12616=DIRECTION('',(1.,0.,0.));
#12617=DIRECTION('center_axis',(-1.,0.,0.));
#12618=DIRECTION('ref_axis',(0.,0.,-1.));
#12619=DIRECTION('center_axis',(1.,0.,0.));
#12620=DIRECTION('ref_axis',(0.,0.,-1.));
#12621=DIRECTION('center_axis',(1.,0.,0.));
#12622=DIRECTION('ref_axis',(0.,0.,-1.));
#12623=DIRECTION('',(1.,0.,0.));
#12624=DIRECTION('center_axis',(-1.,0.,0.));
#12625=DIRECTION('ref_axis',(0.,0.,-1.));
#12626=DIRECTION('center_axis',(1.,0.,0.));
#12627=DIRECTION('ref_axis',(0.,0.,-1.));
#12628=DIRECTION('center_axis',(1.,0.,0.));
#12629=DIRECTION('ref_axis',(0.,0.,-1.));
#12630=DIRECTION('',(1.,0.,0.));
#12631=DIRECTION('center_axis',(-1.,0.,0.));
#12632=DIRECTION('ref_axis',(0.,0.,-1.));
#12633=DIRECTION('center_axis',(1.,0.,0.));
#12634=DIRECTION('ref_axis',(0.,0.,-1.));
#12635=DIRECTION('center_axis',(1.,0.,0.));
#12636=DIRECTION('ref_axis',(0.,0.,-1.));
#12637=DIRECTION('',(1.,0.,0.));
#12638=DIRECTION('center_axis',(-1.,0.,0.));
#12639=DIRECTION('ref_axis',(0.,0.,-1.));
#12640=DIRECTION('center_axis',(1.,0.,0.));
#12641=DIRECTION('ref_axis',(0.,0.,-1.));
#12642=DIRECTION('center_axis',(1.,0.,0.));
#12643=DIRECTION('ref_axis',(0.,0.,-1.));
#12644=DIRECTION('',(1.,0.,0.));
#12645=DIRECTION('center_axis',(-1.,0.,0.));
#12646=DIRECTION('ref_axis',(0.,0.,-1.));
#12647=DIRECTION('center_axis',(0.,1.,0.));
#12648=DIRECTION('ref_axis',(-1.,0.,0.));
#12649=DIRECTION('',(-1.,0.,0.));
#12650=DIRECTION('',(0.,0.,1.));
#12651=DIRECTION('',(-1.,0.,0.));
#12652=DIRECTION('',(0.,0.,1.));
#12653=DIRECTION('center_axis',(1.,0.,0.));
#12654=DIRECTION('ref_axis',(0.,1.,0.));
#12655=DIRECTION('',(0.,1.,0.));
#12656=DIRECTION('',(0.,1.,0.));
#12657=DIRECTION('',(0.,0.,1.));
#12658=DIRECTION('center_axis',(0.,-1.,0.));
#12659=DIRECTION('ref_axis',(1.,0.,0.));
#12660=DIRECTION('',(1.,0.,0.));
#12661=DIRECTION('',(1.,0.,0.));
#12662=DIRECTION('',(0.,0.,1.));
#12663=DIRECTION('center_axis',(-1.,0.,0.));
#12664=DIRECTION('ref_axis',(0.,-1.,0.));
#12665=DIRECTION('',(0.,-1.,0.));
#12666=DIRECTION('',(0.,-1.,0.));
#12667=DIRECTION('center_axis',(0.,0.,1.));
#12668=DIRECTION('ref_axis',(1.,0.,0.));
#12669=DIRECTION('center_axis',(0.,0.,1.));
#12670=DIRECTION('ref_axis',(1.,0.,0.));
#12671=DIRECTION('axis',(0.,0.,1.));
#12672=DIRECTION('refdir',(1.,0.,0.));
#12673=DIRECTION('center_axis',(1.,0.,0.));
#12674=DIRECTION('ref_axis',(0.,0.,-1.));
#12675=DIRECTION('center_axis',(1.,0.,0.));
#12676=DIRECTION('ref_axis',(0.,0.,-1.));
#12677=DIRECTION('',(1.,0.,0.));
#12678=DIRECTION('center_axis',(-1.,0.,0.));
#12679=DIRECTION('ref_axis',(0.,0.,-1.));
#12680=DIRECTION('center_axis',(1.,0.,0.));
#12681=DIRECTION('ref_axis',(0.,0.,-1.));
#12682=DIRECTION('center_axis',(1.,0.,0.));
#12683=DIRECTION('ref_axis',(0.,0.,-1.));
#12684=DIRECTION('',(1.,0.,0.));
#12685=DIRECTION('center_axis',(-1.,0.,0.));
#12686=DIRECTION('ref_axis',(0.,0.,-1.));
#12687=DIRECTION('center_axis',(1.,0.,0.));
#12688=DIRECTION('ref_axis',(0.,0.,-1.));
#12689=DIRECTION('center_axis',(1.,0.,0.));
#12690=DIRECTION('ref_axis',(0.,0.,-1.));
#12691=DIRECTION('',(1.,0.,0.));
#12692=DIRECTION('center_axis',(-1.,0.,0.));
#12693=DIRECTION('ref_axis',(0.,0.,-1.));
#12694=DIRECTION('center_axis',(1.,0.,0.));
#12695=DIRECTION('ref_axis',(0.,0.,-1.));
#12696=DIRECTION('center_axis',(1.,0.,0.));
#12697=DIRECTION('ref_axis',(0.,0.,-1.));
#12698=DIRECTION('',(1.,0.,0.));
#12699=DIRECTION('center_axis',(-1.,0.,0.));
#12700=DIRECTION('ref_axis',(0.,0.,-1.));
#12701=DIRECTION('center_axis',(1.,0.,0.));
#12702=DIRECTION('ref_axis',(0.,0.,-1.));
#12703=DIRECTION('center_axis',(1.,0.,0.));
#12704=DIRECTION('ref_axis',(0.,0.,-1.));
#12705=DIRECTION('',(1.,0.,0.));
#12706=DIRECTION('center_axis',(-1.,0.,0.));
#12707=DIRECTION('ref_axis',(0.,0.,-1.));
#12708=DIRECTION('center_axis',(1.,0.,0.));
#12709=DIRECTION('ref_axis',(0.,0.,-1.));
#12710=DIRECTION('center_axis',(1.,0.,0.));
#12711=DIRECTION('ref_axis',(0.,0.,-1.));
#12712=DIRECTION('',(1.,0.,0.));
#12713=DIRECTION('center_axis',(-1.,0.,0.));
#12714=DIRECTION('ref_axis',(0.,0.,-1.));
#12715=DIRECTION('center_axis',(1.,0.,0.));
#12716=DIRECTION('ref_axis',(0.,0.,-1.));
#12717=DIRECTION('center_axis',(1.,0.,0.));
#12718=DIRECTION('ref_axis',(0.,0.,-1.));
#12719=DIRECTION('',(1.,0.,0.));
#12720=DIRECTION('center_axis',(-1.,0.,0.));
#12721=DIRECTION('ref_axis',(0.,0.,-1.));
#12722=DIRECTION('center_axis',(0.,1.,0.));
#12723=DIRECTION('ref_axis',(-1.,0.,0.));
#12724=DIRECTION('',(-1.,0.,0.));
#12725=DIRECTION('',(0.,0.,1.));
#12726=DIRECTION('',(-1.,0.,0.));
#12727=DIRECTION('',(0.,0.,1.));
#12728=DIRECTION('center_axis',(1.,0.,0.));
#12729=DIRECTION('ref_axis',(0.,1.,0.));
#12730=DIRECTION('',(0.,1.,0.));
#12731=DIRECTION('',(0.,1.,0.));
#12732=DIRECTION('',(0.,0.,1.));
#12733=DIRECTION('center_axis',(0.,-1.,0.));
#12734=DIRECTION('ref_axis',(1.,0.,0.));
#12735=DIRECTION('',(1.,0.,0.));
#12736=DIRECTION('',(1.,0.,0.));
#12737=DIRECTION('',(0.,0.,1.));
#12738=DIRECTION('center_axis',(-1.,0.,0.));
#12739=DIRECTION('ref_axis',(0.,-1.,0.));
#12740=DIRECTION('',(0.,-1.,0.));
#12741=DIRECTION('',(0.,-1.,0.));
#12742=DIRECTION('center_axis',(0.,0.,1.));
#12743=DIRECTION('ref_axis',(1.,0.,0.));
#12744=DIRECTION('center_axis',(0.,0.,1.));
#12745=DIRECTION('ref_axis',(1.,0.,0.));
#12746=DIRECTION('axis',(0.,0.,1.));
#12747=DIRECTION('refdir',(1.,0.,0.));
#12748=DIRECTION('center_axis',(1.,0.,0.));
#12749=DIRECTION('ref_axis',(0.,0.,-1.));
#12750=DIRECTION('center_axis',(1.,0.,0.));
#12751=DIRECTION('ref_axis',(0.,0.,-1.));
#12752=DIRECTION('center_axis',(1.,0.,0.));
#12753=DIRECTION('ref_axis',(0.,0.,-1.));
#12754=DIRECTION('center_axis',(1.,0.,0.));
#12755=DIRECTION('ref_axis',(0.,0.,-1.));
#12756=DIRECTION('center_axis',(1.,0.,0.));
#12757=DIRECTION('ref_axis',(0.,0.,-1.));
#12758=DIRECTION('center_axis',(1.,0.,0.));
#12759=DIRECTION('ref_axis',(0.,0.,-1.));
#12760=DIRECTION('',(1.,0.,0.));
#12761=DIRECTION('',(1.,0.,0.));
#12762=DIRECTION('center_axis',(-1.,0.,0.));
#12763=DIRECTION('ref_axis',(0.,0.,-1.));
#12764=DIRECTION('',(-1.,0.,0.));
#12765=DIRECTION('center_axis',(1.,0.,0.));
#12766=DIRECTION('ref_axis',(0.,0.,-1.));
#12767=DIRECTION('center_axis',(1.,0.,0.));
#12768=DIRECTION('ref_axis',(0.,0.,-1.));
#12769=DIRECTION('center_axis',(1.,0.,0.));
#12770=DIRECTION('ref_axis',(0.,0.,-1.));
#12771=DIRECTION('center_axis',(1.,0.,0.));
#12772=DIRECTION('ref_axis',(0.,0.,-1.));
#12773=DIRECTION('center_axis',(1.,0.,0.));
#12774=DIRECTION('ref_axis',(0.,0.,-1.));
#12775=DIRECTION('center_axis',(1.,0.,0.));
#12776=DIRECTION('ref_axis',(0.,0.,-1.));
#12777=DIRECTION('',(1.,0.,0.));
#12778=DIRECTION('center_axis',(-1.,0.,0.));
#12779=DIRECTION('ref_axis',(0.,0.,-1.));
#12780=DIRECTION('',(-1.,0.,0.));
#12781=DIRECTION('',(1.,0.,0.));
#12782=DIRECTION('center_axis',(-1.,0.,0.));
#12783=DIRECTION('ref_axis',(0.,0.,-1.));
#12784=DIRECTION('center_axis',(1.,0.,0.));
#12785=DIRECTION('ref_axis',(0.,0.,-1.));
#12786=DIRECTION('center_axis',(1.,0.,0.));
#12787=DIRECTION('ref_axis',(0.,0.,-1.));
#12788=DIRECTION('',(-1.,0.,0.));
#12789=DIRECTION('center_axis',(1.,0.,0.));
#12790=DIRECTION('ref_axis',(0.,0.,-1.));
#12791=DIRECTION('center_axis',(1.,0.,0.));
#12792=DIRECTION('ref_axis',(0.,0.,-1.));
#12793=DIRECTION('center_axis',(1.,0.,0.));
#12794=DIRECTION('ref_axis',(0.,0.,-1.));
#12795=DIRECTION('center_axis',(1.,0.,0.));
#12796=DIRECTION('ref_axis',(0.,0.,-1.));
#12797=DIRECTION('center_axis',(1.,0.,0.));
#12798=DIRECTION('ref_axis',(0.,0.,-1.));
#12799=DIRECTION('',(-1.,0.,0.));
#12800=DIRECTION('center_axis',(1.,0.,0.));
#12801=DIRECTION('ref_axis',(0.,0.,-1.));
#12802=DIRECTION('center_axis',(1.,0.,0.));
#12803=DIRECTION('ref_axis',(0.,0.,-1.));
#12804=DIRECTION('center_axis',(-1.,0.,0.));
#12805=DIRECTION('ref_axis',(0.,0.,-1.));
#12806=DIRECTION('center_axis',(1.,0.,0.));
#12807=DIRECTION('ref_axis',(0.,0.,-1.));
#12808=DIRECTION('center_axis',(-1.,0.,0.));
#12809=DIRECTION('ref_axis',(0.,0.,-1.));
#12810=DIRECTION('',(-1.,0.,0.));
#12811=DIRECTION('center_axis',(1.,0.,0.));
#12812=DIRECTION('ref_axis',(0.,0.,-1.));
#12813=DIRECTION('axis',(0.,0.,1.));
#12814=DIRECTION('refdir',(1.,0.,0.));
#12815=DIRECTION('center_axis',(1.,0.,0.));
#12816=DIRECTION('ref_axis',(0.,0.,-1.));
#12817=DIRECTION('center_axis',(1.,0.,0.));
#12818=DIRECTION('ref_axis',(0.,0.,-1.));
#12819=DIRECTION('',(1.,0.,0.));
#12820=DIRECTION('center_axis',(1.,0.,0.));
#12821=DIRECTION('ref_axis',(0.,0.,-1.));
#12822=DIRECTION('center_axis',(1.,0.,0.));
#12823=DIRECTION('ref_axis',(0.,0.,-1.));
#12824=DIRECTION('center_axis',(-1.,0.,0.));
#12825=DIRECTION('ref_axis',(0.,0.,-1.));
#12826=DIRECTION('center_axis',(1.,0.,0.));
#12827=DIRECTION('ref_axis',(0.,0.,-1.));
#12828=DIRECTION('center_axis',(1.,0.,0.));
#12829=DIRECTION('ref_axis',(0.,0.,-1.));
#12830=DIRECTION('',(1.,0.,0.));
#12831=DIRECTION('center_axis',(1.,0.,0.));
#12832=DIRECTION('ref_axis',(0.,0.,-1.));
#12833=DIRECTION('center_axis',(1.,0.,0.));
#12834=DIRECTION('ref_axis',(0.,0.,-1.));
#12835=DIRECTION('center_axis',(-1.,0.,0.));
#12836=DIRECTION('ref_axis',(0.,0.,-1.));
#12837=DIRECTION('center_axis',(1.,0.,0.));
#12838=DIRECTION('ref_axis',(0.,0.,-1.));
#12839=DIRECTION('center_axis',(1.,0.,0.));
#12840=DIRECTION('ref_axis',(0.,0.,-1.));
#12841=DIRECTION('',(1.,0.,0.));
#12842=DIRECTION('center_axis',(1.,0.,0.));
#12843=DIRECTION('ref_axis',(0.,0.,-1.));
#12844=DIRECTION('center_axis',(1.,0.,0.));
#12845=DIRECTION('ref_axis',(0.,0.,-1.));
#12846=DIRECTION('center_axis',(-1.,0.,0.));
#12847=DIRECTION('ref_axis',(0.,0.,-1.));
#12848=DIRECTION('center_axis',(1.,0.,0.));
#12849=DIRECTION('ref_axis',(0.,0.,-1.));
#12850=DIRECTION('center_axis',(1.,0.,0.));
#12851=DIRECTION('ref_axis',(0.,0.,-1.));
#12852=DIRECTION('',(1.,0.,0.));
#12853=DIRECTION('center_axis',(1.,0.,0.));
#12854=DIRECTION('ref_axis',(0.,0.,-1.));
#12855=DIRECTION('center_axis',(1.,0.,0.));
#12856=DIRECTION('ref_axis',(0.,0.,-1.));
#12857=DIRECTION('center_axis',(-1.,0.,0.));
#12858=DIRECTION('ref_axis',(0.,0.,-1.));
#12859=DIRECTION('center_axis',(1.,0.,0.));
#12860=DIRECTION('ref_axis',(0.,0.,-1.));
#12861=DIRECTION('',(1.,0.,0.));
#12862=DIRECTION('center_axis',(-1.,0.,0.));
#12863=DIRECTION('ref_axis',(0.,0.,-1.));
#12864=DIRECTION('center_axis',(1.,0.,0.));
#12865=DIRECTION('ref_axis',(0.,0.,-1.));
#12866=DIRECTION('',(1.,0.,0.));
#12867=DIRECTION('center_axis',(-1.,0.,0.));
#12868=DIRECTION('ref_axis',(0.,0.,-1.));
#12869=DIRECTION('center_axis',(1.,0.,0.));
#12870=DIRECTION('ref_axis',(0.,0.,-1.));
#12871=DIRECTION('',(1.,0.,0.));
#12872=DIRECTION('center_axis',(-1.,0.,0.));
#12873=DIRECTION('ref_axis',(0.,0.,-1.));
#12874=DIRECTION('center_axis',(1.,0.,0.));
#12875=DIRECTION('ref_axis',(0.,0.,-1.));
#12876=DIRECTION('',(1.,0.,0.));
#12877=DIRECTION('center_axis',(-1.,0.,0.));
#12878=DIRECTION('ref_axis',(0.,0.,-1.));
#12879=DIRECTION('center_axis',(0.,1.,0.));
#12880=DIRECTION('ref_axis',(-1.,0.,0.));
#12881=DIRECTION('',(-1.,0.,0.));
#12882=DIRECTION('',(0.,0.,1.));
#12883=DIRECTION('',(-1.,0.,0.));
#12884=DIRECTION('',(0.,0.,1.));
#12885=DIRECTION('center_axis',(1.,0.,0.));
#12886=DIRECTION('ref_axis',(0.,1.,0.));
#12887=DIRECTION('',(0.,1.,0.));
#12888=DIRECTION('',(0.,1.,0.));
#12889=DIRECTION('',(0.,0.,1.));
#12890=DIRECTION('center_axis',(0.,-1.,0.));
#12891=DIRECTION('ref_axis',(1.,0.,0.));
#12892=DIRECTION('',(1.,0.,0.));
#12893=DIRECTION('',(1.,0.,0.));
#12894=DIRECTION('',(0.,0.,1.));
#12895=DIRECTION('center_axis',(-1.,0.,0.));
#12896=DIRECTION('ref_axis',(0.,-1.,0.));
#12897=DIRECTION('',(0.,-1.,0.));
#12898=DIRECTION('',(0.,-1.,0.));
#12899=DIRECTION('center_axis',(0.,0.,1.));
#12900=DIRECTION('ref_axis',(1.,0.,0.));
#12901=DIRECTION('center_axis',(0.,0.,1.));
#12902=DIRECTION('ref_axis',(1.,0.,0.));
#12903=DIRECTION('axis',(0.,0.,1.));
#12904=DIRECTION('refdir',(1.,0.,0.));
#12905=DIRECTION('axis',(0.,0.,1.));
#12906=DIRECTION('refdir',(1.,0.,0.));
#12907=DIRECTION('center_axis',(0.,1.,0.));
#12908=DIRECTION('ref_axis',(0.,0.,1.));
#12909=DIRECTION('center_axis',(0.,-1.,0.));
#12910=DIRECTION('ref_axis',(1.,0.,0.));
#12911=DIRECTION('',(-1.,0.,0.));
#12912=DIRECTION('',(0.,0.,-1.));
#12913=DIRECTION('',(1.,0.,0.));
#12914=DIRECTION('center_axis',(0.,0.,1.));
#12915=DIRECTION('ref_axis',(1.,0.,0.));
#12916=DIRECTION('',(0.,-1.,0.));
#12917=DIRECTION('',(0.,1.,0.));
#12918=DIRECTION('',(-1.,0.,0.));
#12919=DIRECTION('center_axis',(0.,-1.,0.));
#12920=DIRECTION('ref_axis',(0.,0.,-1.));
#12921=DIRECTION('center_axis',(0.,1.,0.));
#12922=DIRECTION('ref_axis',(1.,0.,0.));
#12923=DIRECTION('',(0.,0.,1.));
#12924=DIRECTION('',(1.,0.,0.));
#12925=DIRECTION('center_axis',(0.,0.,-1.));
#12926=DIRECTION('ref_axis',(-1.,0.,0.));
#12927=DIRECTION('',(0.,1.,0.));
#12928=DIRECTION('',(0.,1.,0.));
#12929=DIRECTION('center_axis',(1.,0.,0.));
#12930=DIRECTION('ref_axis',(0.,0.,-1.));
#12931=DIRECTION('center_axis',(0.,1.,0.));
#12932=DIRECTION('ref_axis',(0.,0.,1.));
#12933=DIRECTION('center_axis',(0.,-1.,0.));
#12934=DIRECTION('ref_axis',(1.,0.,0.));
#12935=DIRECTION('center_axis',(0.,-1.,0.));
#12936=DIRECTION('ref_axis',(1.,0.,0.));
#12937=DIRECTION('center_axis',(0.,-1.,0.));
#12938=DIRECTION('ref_axis',(1.,0.,0.));
#12939=DIRECTION('center_axis',(0.,-1.,0.));
#12940=DIRECTION('ref_axis',(1.,0.,0.));
#12941=DIRECTION('',(0.,1.,0.));
#12942=DIRECTION('center_axis',(0.,-1.,0.));
#12943=DIRECTION('ref_axis',(0.,0.,-1.));
#12944=DIRECTION('center_axis',(0.,-1.,0.));
#12945=DIRECTION('ref_axis',(1.,0.,0.));
#12946=DIRECTION('center_axis',(0.,-1.,0.));
#12947=DIRECTION('ref_axis',(1.,0.,0.));
#12948=DIRECTION('center_axis',(0.,-1.,0.));
#12949=DIRECTION('ref_axis',(1.,0.,0.));
#12950=DIRECTION('',(0.,1.,0.));
#12951=DIRECTION('center_axis',(0.,1.,0.));
#12952=DIRECTION('ref_axis',(0.,0.,1.));
#12953=DIRECTION('center_axis',(0.,-1.,0.));
#12954=DIRECTION('ref_axis',(1.,0.,0.));
#12955=DIRECTION('center_axis',(0.,-1.,0.));
#12956=DIRECTION('ref_axis',(1.,0.,0.));
#12957=DIRECTION('center_axis',(0.,-1.,0.));
#12958=DIRECTION('ref_axis',(1.,0.,0.));
#12959=DIRECTION('',(0.,1.,0.));
#12960=DIRECTION('center_axis',(0.,-1.,0.));
#12961=DIRECTION('ref_axis',(0.,0.,-1.));
#12962=DIRECTION('center_axis',(0.,-1.,0.));
#12963=DIRECTION('ref_axis',(1.,0.,0.));
#12964=DIRECTION('center_axis',(0.,-1.,0.));
#12965=DIRECTION('ref_axis',(1.,0.,0.));
#12966=DIRECTION('center_axis',(0.,-1.,0.));
#12967=DIRECTION('ref_axis',(1.,0.,0.));
#12968=DIRECTION('',(0.,1.,0.));
#12969=DIRECTION('center_axis',(0.,1.,0.));
#12970=DIRECTION('ref_axis',(0.,0.,1.));
#12971=DIRECTION('center_axis',(0.,-1.,0.));
#12972=DIRECTION('ref_axis',(1.,0.,0.));
#12973=DIRECTION('center_axis',(0.,-1.,0.));
#12974=DIRECTION('ref_axis',(1.,0.,0.));
#12975=DIRECTION('center_axis',(0.,-1.,0.));
#12976=DIRECTION('ref_axis',(1.,0.,0.));
#12977=DIRECTION('',(0.,1.,0.));
#12978=DIRECTION('center_axis',(0.,-1.,0.));
#12979=DIRECTION('ref_axis',(0.,0.,-1.));
#12980=DIRECTION('center_axis',(0.,-1.,0.));
#12981=DIRECTION('ref_axis',(1.,0.,0.));
#12982=DIRECTION('center_axis',(0.,-1.,0.));
#12983=DIRECTION('ref_axis',(1.,0.,0.));
#12984=DIRECTION('',(0.,1.,0.));
#12985=DIRECTION('axis',(0.,0.,1.));
#12986=DIRECTION('refdir',(1.,0.,0.));
#12987=DIRECTION('center_axis',(0.,1.,0.));
#12988=DIRECTION('ref_axis',(0.,0.,1.));
#12989=DIRECTION('center_axis',(0.,1.,0.));
#12990=DIRECTION('ref_axis',(1.,0.,0.));
#12991=DIRECTION('',(1.,0.,0.));
#12992=DIRECTION('center_axis',(0.,-1.,0.));
#12993=DIRECTION('ref_axis',(1.,0.,0.));
#12994=DIRECTION('',(-1.,0.,0.));
#12995=DIRECTION('center_axis',(0.,0.,-1.));
#12996=DIRECTION('ref_axis',(-1.,0.,0.));
#12997=DIRECTION('',(0.,-1.,0.));
#12998=DIRECTION('',(0.,1.,0.));
#12999=DIRECTION('',(1.,0.,0.));
#13000=DIRECTION('center_axis',(0.,-1.,0.));
#13001=DIRECTION('ref_axis',(0.,0.,-1.));
#13002=DIRECTION('center_axis',(0.,-1.,0.));
#13003=DIRECTION('ref_axis',(1.,0.,0.));
#13004=DIRECTION('center_axis',(0.,1.,0.));
#13005=DIRECTION('ref_axis',(1.,0.,0.));
#13006=DIRECTION('',(-1.,0.,0.));
#13007=DIRECTION('center_axis',(0.,0.,1.));
#13008=DIRECTION('ref_axis',(1.,0.,0.));
#13009=DIRECTION('',(0.,1.,0.));
#13010=DIRECTION('',(0.,-1.,0.));
#13011=DIRECTION('center_axis',(0.,1.,0.));
#13012=DIRECTION('ref_axis',(0.,0.,1.));
#13013=DIRECTION('center_axis',(0.,-1.,0.));
#13014=DIRECTION('ref_axis',(1.,0.,0.));
#13015=DIRECTION('center_axis',(0.,-1.,0.));
#13016=DIRECTION('ref_axis',(1.,0.,0.));
#13017=DIRECTION('center_axis',(0.,-1.,0.));
#13018=DIRECTION('ref_axis',(1.,0.,0.));
#13019=DIRECTION('center_axis',(0.,-1.,0.));
#13020=DIRECTION('ref_axis',(1.,0.,0.));
#13021=DIRECTION('',(0.,1.,0.));
#13022=DIRECTION('center_axis',(0.,-1.,0.));
#13023=DIRECTION('ref_axis',(0.,0.,-1.));
#13024=DIRECTION('center_axis',(0.,-1.,0.));
#13025=DIRECTION('ref_axis',(1.,0.,0.));
#13026=DIRECTION('center_axis',(0.,-1.,0.));
#13027=DIRECTION('ref_axis',(1.,0.,0.));
#13028=DIRECTION('',(0.,1.,0.));
#13029=DIRECTION('',(0.,0.,1.));
#13030=DIRECTION('',(1.,0.,0.));
#13031=DIRECTION('',(0.,0.,1.));
#13032=DIRECTION('',(1.,0.,0.));
#13033=DIRECTION('axis',(0.,0.,1.));
#13034=DIRECTION('refdir',(1.,0.,0.));
#13035=DIRECTION('center_axis',(0.866025403784439,0.,-0.5));
#13036=DIRECTION('ref_axis',(0.5,0.,0.866025403784439));
#13037=DIRECTION('',(-0.5,0.,-0.866025403784439));
#13038=DIRECTION('',(0.,-1.,0.));
#13039=DIRECTION('',(0.5,0.,0.866025403784439));
#13040=DIRECTION('',(0.,-1.,0.));
#13041=DIRECTION('center_axis',(1.60246890531964E-16,0.,-1.));
#13042=DIRECTION('ref_axis',(1.,0.,1.60246890531964E-16));
#13043=DIRECTION('',(-1.,0.,-1.60246890531964E-16));
#13044=DIRECTION('',(0.,-1.,0.));
#13045=DIRECTION('',(1.,0.,1.60246890531964E-16));
#13046=DIRECTION('center_axis',(-0.866025403784439,0.,-0.5));
#13047=DIRECTION('ref_axis',(0.5,0.,-0.866025403784439));
#13048=DIRECTION('',(-0.5,0.,0.866025403784439));
#13049=DIRECTION('',(0.,-1.,0.));
#13050=DIRECTION('',(0.5,0.,-0.866025403784439));
#13051=DIRECTION('center_axis',(-0.866025403784439,0.,0.5));
#13052=DIRECTION('ref_axis',(-0.5,0.,-0.866025403784439));
#13053=DIRECTION('',(0.5,0.,0.866025403784439));
#13054=DIRECTION('',(0.,-1.,0.));
#13055=DIRECTION('',(-0.5,0.,-0.866025403784439));
#13056=DIRECTION('center_axis',(-1.60246890531964E-16,0.,1.));
#13057=DIRECTION('ref_axis',(-1.,0.,-1.60246890531964E-16));
#13058=DIRECTION('',(1.,0.,1.60246890531964E-16));
#13059=DIRECTION('',(0.,-1.,0.));
#13060=DIRECTION('',(-1.,0.,-1.60246890531964E-16));
#13061=DIRECTION('center_axis',(0.866025403784439,0.,0.5));
#13062=DIRECTION('ref_axis',(-0.5,0.,0.866025403784439));
#13063=DIRECTION('',(0.5,0.,-0.866025403784439));
#13064=DIRECTION('',(-0.5,0.,0.866025403784439));
#13065=DIRECTION('center_axis',(0.,1.,0.));
#13066=DIRECTION('ref_axis',(1.,0.,0.));
#13067=DIRECTION('center_axis',(0.,-1.,0.));
#13068=DIRECTION('ref_axis',(0.,0.,-1.));
#13069=DIRECTION('center_axis',(0.,1.,0.));
#13070=DIRECTION('ref_axis',(1.,0.,0.));
#13071=DIRECTION('center_axis',(0.,1.,0.));
#13072=DIRECTION('ref_axis',(1.,0.,0.));
#13073=DIRECTION('center_axis',(0.,1.,0.));
#13074=DIRECTION('ref_axis',(0.,0.,1.));
#13075=DIRECTION('center_axis',(0.,-1.,0.));
#13076=DIRECTION('ref_axis',(1.,0.,0.));
#13077=DIRECTION('center_axis',(0.,-1.,0.));
#13078=DIRECTION('ref_axis',(1.,0.,0.));
#13079=DIRECTION('center_axis',(0.,-1.,0.));
#13080=DIRECTION('ref_axis',(1.,0.,0.));
#13081=DIRECTION('',(0.707106781186547,0.707106781186548,8.65956056235493E-17));
#13082=DIRECTION('center_axis',(0.,-1.,0.));
#13083=DIRECTION('ref_axis',(1.,0.,0.));
#13084=DIRECTION('center_axis',(0.,-1.,0.));
#13085=DIRECTION('ref_axis',(1.,0.,0.));
#13086=DIRECTION('',(0.,1.,0.));
#13087=DIRECTION('center_axis',(0.,1.,0.));
#13088=DIRECTION('ref_axis',(1.,0.,0.));
#13089=DIRECTION('center_axis',(0.,-1.,0.));
#13090=DIRECTION('ref_axis',(1.,0.,0.));
#13091=DIRECTION('',(-0.707106781186547,0.707106781186548,-8.65956056235493E-17));
#13092=DIRECTION('center_axis',(0.,-1.,0.));
#13093=DIRECTION('ref_axis',(0.,0.,-1.));
#13094=DIRECTION('center_axis',(0.,-1.,0.));
#13095=DIRECTION('ref_axis',(1.,0.,0.));
#13096=DIRECTION('center_axis',(0.,1.,0.));
#13097=DIRECTION('ref_axis',(1.,0.,0.));
#13098=DIRECTION('center_axis',(0.,1.,0.));
#13099=DIRECTION('ref_axis',(1.,0.,0.));
#13100=DIRECTION('',(-0.447213595499958,0.894427190999916,-5.47678698264203E-17));
#13101=DIRECTION('center_axis',(0.,-1.,0.));
#13102=DIRECTION('ref_axis',(1.,0.,0.));
#13103=DIRECTION('',(0.,1.,0.));
#13104=DIRECTION('axis',(0.,0.,1.));
#13105=DIRECTION('refdir',(1.,0.,0.));
#13106=DIRECTION('axis',(0.,0.,1.));
#13107=DIRECTION('refdir',(1.,0.,0.));
#13108=DIRECTION('center_axis',(1.,0.,0.));
#13109=DIRECTION('ref_axis',(0.,0.,-1.));
#13110=DIRECTION('center_axis',(1.,0.,0.));
#13111=DIRECTION('ref_axis',(0.,0.,-1.));
#13112=DIRECTION('',(1.,0.,0.));
#13113=DIRECTION('center_axis',(-1.,0.,0.));
#13114=DIRECTION('ref_axis',(0.,0.,-1.));
#13115=DIRECTION('center_axis',(1.,0.,0.));
#13116=DIRECTION('ref_axis',(0.,0.,-1.));
#13117=DIRECTION('center_axis',(1.,0.,0.));
#13118=DIRECTION('ref_axis',(0.,0.,-1.));
#13119=DIRECTION('center_axis',(1.,0.,0.));
#13120=DIRECTION('ref_axis',(0.,0.,-1.));
#13121=DIRECTION('',(1.,0.,0.));
#13122=DIRECTION('center_axis',(1.,0.,0.));
#13123=DIRECTION('ref_axis',(0.,0.,-1.));
#13124=DIRECTION('center_axis',(1.,0.,0.));
#13125=DIRECTION('ref_axis',(0.,0.,-1.));
#13126=DIRECTION('center_axis',(1.,0.,0.));
#13127=DIRECTION('ref_axis',(0.,0.,-1.));
#13128=DIRECTION('center_axis',(1.,0.,0.));
#13129=DIRECTION('ref_axis',(0.,0.,-1.));
#13130=DIRECTION('center_axis',(1.,0.,0.));
#13131=DIRECTION('ref_axis',(0.,0.,-1.));
#13132=DIRECTION('center_axis',(1.,0.,0.));
#13133=DIRECTION('ref_axis',(0.,0.,-1.));
#13134=DIRECTION('center_axis',(1.,0.,0.));
#13135=DIRECTION('ref_axis',(0.,0.,-1.));
#13136=DIRECTION('center_axis',(-1.,0.,0.));
#13137=DIRECTION('ref_axis',(0.,0.,-1.));
#13138=DIRECTION('center_axis',(1.,0.,0.));
#13139=DIRECTION('ref_axis',(0.,0.,-1.));
#13140=DIRECTION('',(-1.,0.,0.));
#13141=DIRECTION('center_axis',(1.,0.,0.));
#13142=DIRECTION('ref_axis',(0.,0.,-1.));
#13143=DIRECTION('',(-1.,0.,0.));
#13144=DIRECTION('center_axis',(1.,0.,0.));
#13145=DIRECTION('ref_axis',(0.,0.,-1.));
#13146=DIRECTION('center_axis',(1.,0.,0.));
#13147=DIRECTION('ref_axis',(0.,0.,-1.));
#13148=DIRECTION('center_axis',(1.,0.,0.));
#13149=DIRECTION('ref_axis',(0.,0.,-1.));
#13150=DIRECTION('center_axis',(1.,0.,0.));
#13151=DIRECTION('ref_axis',(0.,0.,-1.));
#13152=DIRECTION('center_axis',(1.,0.,0.));
#13153=DIRECTION('ref_axis',(0.,0.,-1.));
#13154=DIRECTION('center_axis',(-1.,0.,0.));
#13155=DIRECTION('ref_axis',(0.,0.,-1.));
#13156=DIRECTION('center_axis',(1.,0.,0.));
#13157=DIRECTION('ref_axis',(0.,0.,-1.));
#13158=DIRECTION('',(-1.,0.,0.));
#13159=DIRECTION('center_axis',(1.,0.,0.));
#13160=DIRECTION('ref_axis',(0.,0.,-1.));
#13161=DIRECTION('',(-1.,0.,0.));
#13162=DIRECTION('center_axis',(1.,0.,0.));
#13163=DIRECTION('ref_axis',(0.,0.,-1.));
#13164=DIRECTION('center_axis',(1.,0.,0.));
#13165=DIRECTION('ref_axis',(0.,0.,-1.));
#13166=DIRECTION('center_axis',(1.,0.,0.));
#13167=DIRECTION('ref_axis',(0.,0.,-1.));
#13168=DIRECTION('',(-1.,0.,0.));
#13169=DIRECTION('center_axis',(1.,0.,0.));
#13170=DIRECTION('ref_axis',(0.,0.,-1.));
#13171=DIRECTION('center_axis',(1.,0.,0.));
#13172=DIRECTION('ref_axis',(0.,0.,-1.));
#13173=DIRECTION('axis',(0.,0.,1.));
#13174=DIRECTION('refdir',(1.,0.,0.));
#13175=DIRECTION('center_axis',(1.,0.,0.));
#13176=DIRECTION('ref_axis',(0.,0.,-1.));
#13177=DIRECTION('center_axis',(-1.,0.,0.));
#13178=DIRECTION('ref_axis',(0.,0.,-1.));
#13179=DIRECTION('',(-1.,0.,0.));
#13180=DIRECTION('center_axis',(-1.,0.,0.));
#13181=DIRECTION('ref_axis',(0.,0.,-1.));
#13182=DIRECTION('center_axis',(1.,0.,0.));
#13183=DIRECTION('ref_axis',(0.,0.,-1.));
#13184=DIRECTION('center_axis',(1.,0.,0.));
#13185=DIRECTION('ref_axis',(0.,0.,-1.));
#13186=DIRECTION('',(-1.,0.,0.));
#13187=DIRECTION('center_axis',(1.,0.,0.));
#13188=DIRECTION('ref_axis',(0.,0.,-1.));
#13189=DIRECTION('center_axis',(1.,0.,0.));
#13190=DIRECTION('ref_axis',(0.,0.,-1.));
#13191=DIRECTION('center_axis',(1.,0.,0.));
#13192=DIRECTION('ref_axis',(0.,0.,-1.));
#13193=DIRECTION('axis',(0.,0.,1.));
#13194=DIRECTION('refdir',(1.,0.,0.));
#13195=DIRECTION('center_axis',(1.,0.,0.));
#13196=DIRECTION('ref_axis',(0.,0.,-1.));
#13197=DIRECTION('center_axis',(-1.,0.,0.));
#13198=DIRECTION('ref_axis',(0.,0.,-1.));
#13199=DIRECTION('',(-1.,0.,0.));
#13200=DIRECTION('center_axis',(-1.,0.,0.));
#13201=DIRECTION('ref_axis',(0.,0.,-1.));
#13202=DIRECTION('center_axis',(1.,0.,0.));
#13203=DIRECTION('ref_axis',(0.,0.,-1.));
#13204=DIRECTION('center_axis',(1.,0.,0.));
#13205=DIRECTION('ref_axis',(0.,0.,-1.));
#13206=DIRECTION('',(-1.,0.,0.));
#13207=DIRECTION('center_axis',(1.,0.,0.));
#13208=DIRECTION('ref_axis',(0.,0.,-1.));
#13209=DIRECTION('center_axis',(1.,0.,0.));
#13210=DIRECTION('ref_axis',(0.,0.,-1.));
#13211=DIRECTION('center_axis',(1.,0.,0.));
#13212=DIRECTION('ref_axis',(0.,0.,-1.));
#13213=DIRECTION('axis',(0.,0.,1.));
#13214=DIRECTION('refdir',(1.,0.,0.));
#13215=DIRECTION('center_axis',(1.,0.,0.));
#13216=DIRECTION('ref_axis',(0.,0.,-1.));
#13217=DIRECTION('center_axis',(-1.,0.,0.));
#13218=DIRECTION('ref_axis',(0.,0.,-1.));
#13219=DIRECTION('',(1.,0.,0.));
#13220=DIRECTION('center_axis',(1.,0.,0.));
#13221=DIRECTION('ref_axis',(0.,0.,-1.));
#13222=DIRECTION('center_axis',(0.,0.,1.));
#13223=DIRECTION('ref_axis',(1.,0.,0.));
#13224=DIRECTION('',(1.,0.,0.));
#13225=DIRECTION('center_axis',(0.,0.,1.));
#13226=DIRECTION('ref_axis',(1.,0.,0.));
#13227=DIRECTION('center_axis',(0.,0.,1.));
#13228=DIRECTION('ref_axis',(1.,0.,0.));
#13229=DIRECTION('center_axis',(0.,0.,1.));
#13230=DIRECTION('ref_axis',(1.,0.,0.));
#13231=DIRECTION('',(0.,0.,1.));
#13232=DIRECTION('center_axis',(0.,0.,1.));
#13233=DIRECTION('ref_axis',(1.,0.,0.));
#13234=DIRECTION('',(-1.,0.,0.));
#13235=DIRECTION('center_axis',(1.,0.,0.));
#13236=DIRECTION('ref_axis',(0.,0.,-1.));
#13237=DIRECTION('center_axis',(1.,0.,0.));
#13238=DIRECTION('ref_axis',(0.,0.,-1.));
#13239=DIRECTION('center_axis',(1.,0.,0.));
#13240=DIRECTION('ref_axis',(0.,0.,-1.));
#13241=DIRECTION('center_axis',(-1.,0.,0.));
#13242=DIRECTION('ref_axis',(0.,0.,-1.));
#13243=DIRECTION('',(-1.,0.,0.));
#13244=DIRECTION('',(-1.,0.,0.));
#13245=DIRECTION('center_axis',(-1.,0.,0.));
#13246=DIRECTION('ref_axis',(0.,0.,-1.));
#13247=DIRECTION('center_axis',(1.,0.,0.));
#13248=DIRECTION('ref_axis',(0.,0.,-1.));
#13249=DIRECTION('center_axis',(1.,0.,0.));
#13250=DIRECTION('ref_axis',(0.,0.,-1.));
#13251=DIRECTION('',(-1.,0.,0.));
#13252=DIRECTION('',(-1.,0.,0.));
#13253=DIRECTION('center_axis',(1.,0.,0.));
#13254=DIRECTION('ref_axis',(0.,0.,-1.));
#13255=DIRECTION('center_axis',(1.,0.,0.));
#13256=DIRECTION('ref_axis',(0.,0.,-1.));
#13257=DIRECTION('axis',(0.,0.,1.));
#13258=DIRECTION('refdir',(1.,0.,0.));
#13259=DIRECTION('center_axis',(1.,0.,0.));
#13260=DIRECTION('ref_axis',(0.,0.,-1.));
#13261=DIRECTION('center_axis',(-1.,0.,0.));
#13262=DIRECTION('ref_axis',(0.,0.,-1.));
#13263=DIRECTION('',(-1.,0.,0.));
#13264=DIRECTION('center_axis',(-1.,0.,0.));
#13265=DIRECTION('ref_axis',(0.,0.,-1.));
#13266=DIRECTION('center_axis',(1.,0.,0.));
#13267=DIRECTION('ref_axis',(0.,0.,-1.));
#13268=DIRECTION('center_axis',(1.,0.,0.));
#13269=DIRECTION('ref_axis',(0.,0.,-1.));
#13270=DIRECTION('',(-1.,0.,0.));
#13271=DIRECTION('center_axis',(1.,0.,0.));
#13272=DIRECTION('ref_axis',(0.,0.,-1.));
#13273=DIRECTION('center_axis',(1.,0.,0.));
#13274=DIRECTION('ref_axis',(0.,0.,-1.));
#13275=DIRECTION('center_axis',(1.,0.,0.));
#13276=DIRECTION('ref_axis',(0.,0.,-1.));
#13277=DIRECTION('axis',(0.,0.,1.));
#13278=DIRECTION('refdir',(1.,0.,0.));
#13279=DIRECTION('center_axis',(1.,0.,0.));
#13280=DIRECTION('ref_axis',(0.,0.,-1.));
#13281=DIRECTION('center_axis',(-1.,0.,0.));
#13282=DIRECTION('ref_axis',(0.,0.,-1.));
#13283=DIRECTION('',(-1.,0.,0.));
#13284=DIRECTION('center_axis',(-1.,0.,0.));
#13285=DIRECTION('ref_axis',(0.,0.,-1.));
#13286=DIRECTION('center_axis',(1.,0.,0.));
#13287=DIRECTION('ref_axis',(0.,0.,-1.));
#13288=DIRECTION('center_axis',(1.,0.,0.));
#13289=DIRECTION('ref_axis',(0.,0.,-1.));
#13290=DIRECTION('',(-1.,0.,0.));
#13291=DIRECTION('center_axis',(1.,0.,0.));
#13292=DIRECTION('ref_axis',(0.,0.,-1.));
#13293=DIRECTION('center_axis',(1.,0.,0.));
#13294=DIRECTION('ref_axis',(0.,0.,-1.));
#13295=DIRECTION('center_axis',(1.,0.,0.));
#13296=DIRECTION('ref_axis',(0.,0.,-1.));
#13297=DIRECTION('axis',(0.,0.,1.));
#13298=DIRECTION('refdir',(1.,0.,0.));
#13299=DIRECTION('center_axis',(0.,0.,1.));
#13300=DIRECTION('ref_axis',(1.,0.,0.));
#13301=DIRECTION('',(1.,0.,0.));
#13302=DIRECTION('center_axis',(0.,0.,1.));
#13303=DIRECTION('ref_axis',(1.,0.,0.));
#13304=DIRECTION('center_axis',(0.,0.,1.));
#13305=DIRECTION('ref_axis',(1.,0.,0.));
#13306=DIRECTION('center_axis',(0.,0.,1.));
#13307=DIRECTION('ref_axis',(1.,0.,0.));
#13308=DIRECTION('',(0.,0.,1.));
#13309=DIRECTION('center_axis',(0.,0.,1.));
#13310=DIRECTION('ref_axis',(1.,0.,0.));
#13311=DIRECTION('',(-1.,0.,0.));
#13312=DIRECTION('center_axis',(1.,0.,0.));
#13313=DIRECTION('ref_axis',(0.,0.,-1.));
#13314=DIRECTION('center_axis',(-1.,0.,0.));
#13315=DIRECTION('ref_axis',(0.,0.,-1.));
#13316=DIRECTION('',(-1.,0.,0.));
#13317=DIRECTION('',(-1.,0.,0.));
#13318=DIRECTION('center_axis',(-1.,0.,0.));
#13319=DIRECTION('ref_axis',(0.,0.,-1.));
#13320=DIRECTION('center_axis',(1.,0.,0.));
#13321=DIRECTION('ref_axis',(0.,0.,-1.));
#13322=DIRECTION('center_axis',(1.,0.,0.));
#13323=DIRECTION('ref_axis',(0.,0.,-1.));
#13324=DIRECTION('',(-1.,0.,0.));
#13325=DIRECTION('',(-1.,0.,0.));
#13326=DIRECTION('center_axis',(1.,0.,0.));
#13327=DIRECTION('ref_axis',(0.,0.,-1.));
#13328=DIRECTION('center_axis',(1.,0.,0.));
#13329=DIRECTION('ref_axis',(0.,0.,-1.));
#13330=DIRECTION('center_axis',(1.,0.,0.));
#13331=DIRECTION('ref_axis',(0.,0.,-1.));
#13332=DIRECTION('axis',(0.,0.,1.));
#13333=DIRECTION('refdir',(1.,0.,0.));
#13334=DIRECTION('center_axis',(0.,1.,0.));
#13335=DIRECTION('ref_axis',(0.,0.,1.));
#13336=DIRECTION('center_axis',(0.,-1.,0.));
#13337=DIRECTION('ref_axis',(1.,0.,0.));
#13338=DIRECTION('center_axis',(0.,-1.,0.));
#13339=DIRECTION('ref_axis',(1.,0.,0.));
#13340=DIRECTION('center_axis',(0.,-1.,0.));
#13341=DIRECTION('ref_axis',(1.,0.,0.));
#13342=DIRECTION('',(0.707106781186547,0.707106781186548,8.65956056235493E-17));
#13343=DIRECTION('center_axis',(0.,-1.,0.));
#13344=DIRECTION('ref_axis',(1.,0.,0.));
#13345=DIRECTION('center_axis',(0.,-1.,0.));
#13346=DIRECTION('ref_axis',(1.,0.,0.));
#13347=DIRECTION('',(0.,1.,0.));
#13348=DIRECTION('center_axis',(0.,1.,0.));
#13349=DIRECTION('ref_axis',(1.,0.,0.));
#13350=DIRECTION('center_axis',(0.,-1.,0.));
#13351=DIRECTION('ref_axis',(1.,0.,0.));
#13352=DIRECTION('',(-0.707106781186547,0.707106781186548,-8.65956056235493E-17));
#13353=DIRECTION('center_axis',(0.,-1.,0.));
#13354=DIRECTION('ref_axis',(0.,0.,-1.));
#13355=DIRECTION('center_axis',(0.,-1.,0.));
#13356=DIRECTION('ref_axis',(1.,0.,0.));
#13357=DIRECTION('center_axis',(0.,1.,0.));
#13358=DIRECTION('ref_axis',(1.,0.,0.));
#13359=DIRECTION('center_axis',(0.,1.,0.));
#13360=DIRECTION('ref_axis',(1.,0.,0.));
#13361=DIRECTION('',(-0.447213595499958,0.894427190999916,-5.47678698264203E-17));
#13362=DIRECTION('center_axis',(0.,-1.,0.));
#13363=DIRECTION('ref_axis',(1.,0.,0.));
#13364=DIRECTION('center_axis',(0.,1.,0.));
#13365=DIRECTION('ref_axis',(1.,0.,0.));
#13366=DIRECTION('',(0.,1.,0.));
#13367=DIRECTION('center_axis',(0.,1.,0.));
#13368=DIRECTION('ref_axis',(1.,0.,0.));
#13369=DIRECTION('center_axis',(0.,-1.,0.));
#13370=DIRECTION('ref_axis',(1.,0.,0.));
#13371=DIRECTION('',(-0.707106781186547,0.707106781186548,-8.65956056235493E-17));
#13372=DIRECTION('center_axis',(0.,-1.,0.));
#13373=DIRECTION('ref_axis',(0.,0.,-1.));
#13374=DIRECTION('center_axis',(0.866025403784439,0.,-0.5));
#13375=DIRECTION('ref_axis',(0.5,0.,0.866025403784439));
#13376=DIRECTION('',(-0.5,0.,-0.866025403784439));
#13377=DIRECTION('',(0.,-1.,0.));
#13378=DIRECTION('',(0.5,0.,0.866025403784439));
#13379=DIRECTION('',(0.,-1.,0.));
#13380=DIRECTION('center_axis',(1.60246890531964E-16,0.,-1.));
#13381=DIRECTION('ref_axis',(1.,0.,1.60246890531964E-16));
#13382=DIRECTION('',(-1.,0.,-1.60246890531964E-16));
#13383=DIRECTION('',(0.,-1.,0.));
#13384=DIRECTION('',(1.,0.,1.60246890531964E-16));
#13385=DIRECTION('center_axis',(-0.866025403784439,0.,-0.5));
#13386=DIRECTION('ref_axis',(0.5,0.,-0.866025403784439));
#13387=DIRECTION('',(-0.5,0.,0.866025403784439));
#13388=DIRECTION('',(0.,-1.,0.));
#13389=DIRECTION('',(0.5,0.,-0.866025403784439));
#13390=DIRECTION('center_axis',(-0.866025403784439,0.,0.5));
#13391=DIRECTION('ref_axis',(-0.5,0.,-0.866025403784439));
#13392=DIRECTION('',(0.5,0.,0.866025403784439));
#13393=DIRECTION('',(0.,-1.,0.));
#13394=DIRECTION('',(-0.5,0.,-0.866025403784439));
#13395=DIRECTION('center_axis',(-1.60246890531964E-16,0.,1.));
#13396=DIRECTION('ref_axis',(-1.,0.,-1.60246890531964E-16));
#13397=DIRECTION('',(1.,0.,1.60246890531964E-16));
#13398=DIRECTION('',(0.,-1.,0.));
#13399=DIRECTION('',(-1.,0.,-1.60246890531964E-16));
#13400=DIRECTION('center_axis',(0.866025403784439,0.,0.5));
#13401=DIRECTION('ref_axis',(-0.5,0.,0.866025403784439));
#13402=DIRECTION('',(0.5,0.,-0.866025403784439));
#13403=DIRECTION('',(-0.5,0.,0.866025403784439));
#13404=DIRECTION('center_axis',(0.,1.,0.));
#13405=DIRECTION('ref_axis',(1.,0.,0.));
#13406=DIRECTION('center_axis',(0.,-1.,0.));
#13407=DIRECTION('ref_axis',(0.,0.,-1.));
#13408=DIRECTION('',(0.,0.,1.));
#13409=DIRECTION('',(1.,0.,0.));
#13410=DIRECTION('',(0.,0.,1.));
#13411=DIRECTION('',(1.,0.,0.));
#13412=DIRECTION('',(0.,0.,1.));
#13413=DIRECTION('',(1.,0.,0.));
#13414=DIRECTION('',(0.,0.,1.));
#13415=DIRECTION('',(1.,0.,0.));
#13416=DIRECTION('',(0.,0.,1.));
#13417=DIRECTION('',(1.,0.,0.));
#13418=DIRECTION('',(0.,0.,1.));
#13419=DIRECTION('',(2.22044604925031E-16,-1.,0.));
#13420=DIRECTION('',(0.,0.,1.));
#13421=DIRECTION('',(2.22044604925031E-16,-1.,0.));
#13422=DIRECTION('',(0.,0.,1.));
#13423=DIRECTION('',(2.22044604925031E-16,1.,0.));
#13424=DIRECTION('',(0.,0.,1.));
#13425=DIRECTION('',(2.22044604925031E-16,1.,0.));
#13426=DIRECTION('',(0.,0.,1.));
#13427=DIRECTION('',(2.22044604925031E-16,1.,0.));
#13428=DIRECTION('',(0.,0.,1.));
#13429=DIRECTION('',(2.22044604925031E-16,1.,0.));
#13430=DIRECTION('',(0.,0.,1.));
#13431=DIRECTION('',(2.22044604925031E-16,-1.,0.));
#13432=DIRECTION('',(0.,0.,1.));
#13433=DIRECTION('',(2.22044604925031E-16,-1.,0.));
#13434=DIRECTION('',(0.,0.,1.));
#13435=DIRECTION('',(2.22044604925031E-16,-1.,0.));
#13436=DIRECTION('',(0.,0.,1.));
#13437=DIRECTION('',(2.22044604925031E-16,-1.,0.));
#13438=DIRECTION('',(0.,0.,1.));
#13439=DIRECTION('',(2.22044604925031E-16,-1.,0.));
#13440=DIRECTION('',(0.,0.,1.));
#13441=DIRECTION('',(2.22044604925031E-16,-1.,0.));
#13442=DIRECTION('',(0.,0.,1.));
#13443=DIRECTION('',(2.22044604925031E-16,-1.,0.));
#13444=DIRECTION('',(0.,0.,1.));
#13445=DIRECTION('',(2.22044604925031E-16,-1.,0.));
#13446=DIRECTION('',(0.,0.,1.));
#13447=DIRECTION('',(2.22044604925031E-16,-1.,0.));
#13448=DIRECTION('',(0.,0.,1.));
#13449=DIRECTION('',(2.22044604925031E-16,-1.,0.));
#13450=DIRECTION('',(0.,0.,1.));
#13451=DIRECTION('',(1.,0.,0.));
#13452=DIRECTION('',(0.,0.,1.));
#13453=DIRECTION('',(1.,0.,0.));
#13454=DIRECTION('',(0.,0.,1.));
#13455=DIRECTION('',(1.,0.,0.));
#13456=DIRECTION('',(0.,0.,1.));
#13457=DIRECTION('',(1.,0.,0.));
#13458=DIRECTION('',(0.,0.,1.));
#13459=DIRECTION('',(1.,0.,0.));
#13460=DIRECTION('',(0.,0.,1.));
#13461=DIRECTION('',(2.22044604925031E-16,-1.,0.));
#13462=DIRECTION('',(0.,0.,1.));
#13463=DIRECTION('',(2.22044604925031E-16,-1.,0.));
#13464=DIRECTION('',(0.,0.,1.));
#13465=DIRECTION('',(2.22044604925031E-16,1.,0.));
#13466=DIRECTION('',(0.,0.,1.));
#13467=DIRECTION('',(2.22044604925031E-16,1.,0.));
#13468=DIRECTION('',(0.,0.,1.));
#13469=DIRECTION('',(2.22044604925031E-16,1.,0.));
#13470=DIRECTION('',(0.,0.,1.));
#13471=DIRECTION('',(2.22044604925031E-16,1.,0.));
#13472=DIRECTION('',(0.,0.,1.));
#13473=DIRECTION('',(2.22044604925031E-16,-1.,0.));
#13474=DIRECTION('',(0.,0.,1.));
#13475=DIRECTION('',(2.22044604925031E-16,-1.,0.));
#13476=DIRECTION('',(0.,0.,1.));
#13477=DIRECTION('',(2.22044604925031E-16,-1.,0.));
#13478=DIRECTION('',(0.,0.,1.));
#13479=DIRECTION('',(2.22044604925031E-16,-1.,0.));
#13480=DIRECTION('',(0.,0.,1.));
#13481=DIRECTION('',(2.22044604925031E-16,1.,0.));
#13482=DIRECTION('',(0.,0.,1.));
#13483=DIRECTION('',(2.22044604925031E-16,1.,0.));
#13484=DIRECTION('',(0.,0.,1.));
#13485=DIRECTION('',(2.22044604925031E-16,1.,0.));
#13486=DIRECTION('',(0.,0.,1.));
#13487=DIRECTION('',(2.22044604925031E-16,1.,0.));
#13488=DIRECTION('',(0.,0.,1.));
#13489=DIRECTION('',(2.22044604925031E-16,1.,0.));
#13490=DIRECTION('',(0.,0.,1.));
#13491=DIRECTION('',(2.22044604925031E-16,1.,0.));
#13492=DIRECTION('axis',(0.,0.,1.));
#13493=DIRECTION('refdir',(1.,0.,0.));
#13494=DIRECTION('center_axis',(0.866025403784439,0.,-0.5));
#13495=DIRECTION('ref_axis',(0.5,0.,0.866025403784439));
#13496=DIRECTION('',(0.5,0.,0.866025403784439));
#13497=DIRECTION('',(0.,-1.,0.));
#13498=DIRECTION('',(0.5,0.,0.866025403784439));
#13499=DIRECTION('',(0.,-1.,0.));
#13500=DIRECTION('center_axis',(1.20185167898973E-16,0.,-1.));
#13501=DIRECTION('ref_axis',(1.,0.,1.20185167898973E-16));
#13502=DIRECTION('',(1.,0.,1.20185167898973E-16));
#13503=DIRECTION('',(0.,-1.,0.));
#13504=DIRECTION('',(1.,0.,1.20185167898973E-16));
#13505=DIRECTION('center_axis',(-0.866025403784439,0.,-0.5));
#13506=DIRECTION('ref_axis',(0.5,0.,-0.866025403784439));
#13507=DIRECTION('',(0.5,0.,-0.866025403784439));
#13508=DIRECTION('',(0.,-1.,0.));
#13509=DIRECTION('',(0.5,0.,-0.866025403784439));
#13510=DIRECTION('center_axis',(-0.866025403784439,0.,0.5));
#13511=DIRECTION('ref_axis',(-0.5,0.,-0.866025403784439));
#13512=DIRECTION('',(-0.5,0.,-0.866025403784439));
#13513=DIRECTION('',(0.,-1.,0.));
#13514=DIRECTION('',(-0.5,0.,-0.866025403784439));
#13515=DIRECTION('center_axis',(-2.40370335797945E-16,0.,1.));
#13516=DIRECTION('ref_axis',(-1.,0.,-2.40370335797945E-16));
#13517=DIRECTION('',(-1.,0.,-2.40370335797945E-16));
#13518=DIRECTION('',(0.,-1.,0.));
#13519=DIRECTION('',(-1.,0.,-2.40370335797945E-16));
#13520=DIRECTION('center_axis',(0.866025403784439,0.,0.5));
#13521=DIRECTION('ref_axis',(-0.5,0.,0.866025403784439));
#13522=DIRECTION('',(-0.5,0.,0.866025403784439));
#13523=DIRECTION('',(-0.5,0.,0.866025403784439));
#13524=DIRECTION('center_axis',(0.,-1.,0.));
#13525=DIRECTION('ref_axis',(0.,0.,-1.));
#13526=DIRECTION('center_axis',(0.,1.,0.));
#13527=DIRECTION('ref_axis',(0.,0.,1.));
#13528=DIRECTION('center_axis',(0.,-1.,0.));
#13529=DIRECTION('ref_axis',(1.,0.,0.));
#13530=DIRECTION('center_axis',(0.,-1.,0.));
#13531=DIRECTION('ref_axis',(1.,0.,0.));
#13532=DIRECTION('center_axis',(0.,-1.,0.));
#13533=DIRECTION('ref_axis',(1.,0.,0.));
#13534=DIRECTION('',(0.707106781186548,0.707106781186547,8.65956056235494E-17));
#13535=DIRECTION('center_axis',(0.,-1.,0.));
#13536=DIRECTION('ref_axis',(1.,0.,0.));
#13537=DIRECTION('center_axis',(0.,1.,0.));
#13538=DIRECTION('ref_axis',(1.,0.,0.));
#13539=DIRECTION('',(0.,1.,0.));
#13540=DIRECTION('center_axis',(0.,1.,0.));
#13541=DIRECTION('ref_axis',(1.,0.,0.));
#13542=DIRECTION('center_axis',(0.,-1.,0.));
#13543=DIRECTION('ref_axis',(1.,0.,0.));
#13544=DIRECTION('',(-0.707106781186548,0.707106781186547,-8.65956056235494E-17));
#13545=DIRECTION('center_axis',(0.,-1.,0.));
#13546=DIRECTION('ref_axis',(0.,0.,-1.));
#13547=DIRECTION('',(0.,0.,1.));
#13548=DIRECTION('',(1.,0.,0.));
#13549=DIRECTION('',(0.,0.,1.));
#13550=DIRECTION('',(1.,0.,0.));
#13551=DIRECTION('',(0.,0.,1.));
#13552=DIRECTION('',(1.,0.,0.));
#13553=DIRECTION('',(0.,0.,1.));
#13554=DIRECTION('',(1.,0.,0.));
#13555=DIRECTION('',(0.,0.,1.));
#13556=DIRECTION('',(1.,0.,0.));
#13557=DIRECTION('',(0.,0.,1.));
#13558=DIRECTION('',(1.,0.,0.));
#13559=DIRECTION('',(0.,0.,1.));
#13560=DIRECTION('',(1.,0.,0.));
#13561=DIRECTION('',(0.,0.,1.));
#13562=DIRECTION('',(1.,0.,0.));
#13563=DIRECTION('',(0.,0.,1.));
#13564=DIRECTION('',(1.,0.,0.));
#13565=DIRECTION('',(0.,0.,1.));
#13566=DIRECTION('',(1.,0.,0.));
#13567=DIRECTION('',(0.,0.,1.));
#13568=DIRECTION('',(1.,0.,0.));
#13569=DIRECTION('',(0.,0.,1.));
#13570=DIRECTION('',(1.,0.,0.));
#13571=DIRECTION('',(0.,0.,1.));
#13572=DIRECTION('',(1.,0.,0.));
#13573=DIRECTION('',(0.,0.,1.));
#13574=DIRECTION('',(1.,0.,0.));
#13575=DIRECTION('',(0.,-1.,2.22044604925031E-16));
#13576=DIRECTION('',(1.,0.,0.));
#13577=DIRECTION('',(0.,-1.,2.22044604925031E-16));
#13578=DIRECTION('',(1.,0.,0.));
#13579=DIRECTION('',(0.,-1.,2.22044604925031E-16));
#13580=DIRECTION('',(1.,0.,0.));
#13581=DIRECTION('',(0.,-1.,2.22044604925031E-16));
#13582=DIRECTION('',(1.,0.,0.));
#13583=DIRECTION('',(0.,-1.,2.22044604925031E-16));
#13584=DIRECTION('',(1.,0.,0.));
#13585=DIRECTION('',(0.,-1.,2.22044604925031E-16));
#13586=DIRECTION('',(1.,0.,0.));
#13587=DIRECTION('',(0.,0.,1.));
#13588=DIRECTION('',(1.,0.,0.));
#13589=DIRECTION('',(0.,-1.,2.22044604925031E-16));
#13590=DIRECTION('',(1.,0.,0.));
#13591=DIRECTION('',(0.,-1.,2.22044604925031E-16));
#13592=DIRECTION('',(1.,0.,0.));
#13593=DIRECTION('',(0.,-1.,2.22044604925031E-16));
#13594=DIRECTION('',(1.,0.,0.));
#13595=DIRECTION('',(0.,-1.,2.22044604925031E-16));
#13596=DIRECTION('',(1.,0.,0.));
#13597=DIRECTION('',(0.,-1.,2.22044604925031E-16));
#13598=DIRECTION('',(1.,0.,0.));
#13599=DIRECTION('',(0.,-1.,2.22044604925031E-16));
#13600=DIRECTION('',(1.,0.,0.));
#13601=DIRECTION('',(0.,-1.,2.22044604925031E-16));
#13602=DIRECTION('',(1.,0.,0.));
#13603=DIRECTION('',(0.,-1.,2.22044604925031E-16));
#13604=DIRECTION('',(1.,0.,0.));
#13605=DIRECTION('',(0.,0.,1.));
#13606=DIRECTION('',(2.22044604925031E-16,-1.,0.));
#13607=DIRECTION('',(0.,0.,1.));
#13608=DIRECTION('',(2.22044604925031E-16,1.,0.));
#13609=DIRECTION('',(0.,0.,1.));
#13610=DIRECTION('',(2.22044604925031E-16,1.,0.));
#13611=DIRECTION('',(0.,0.,1.));
#13612=DIRECTION('',(2.22044604925031E-16,1.,0.));
#13613=DIRECTION('',(0.,0.,1.));
#13614=DIRECTION('',(2.22044604925031E-16,1.,0.));
#13615=DIRECTION('',(0.,0.,1.));
#13616=DIRECTION('',(2.22044604925031E-16,-1.,0.));
#13617=DIRECTION('',(0.,0.,1.));
#13618=DIRECTION('',(2.22044604925031E-16,-1.,0.));
#13619=DIRECTION('',(0.,0.,1.));
#13620=DIRECTION('',(2.22044604925031E-16,-1.,0.));
#13621=DIRECTION('',(0.,0.,1.));
#13622=DIRECTION('',(2.22044604925031E-16,-1.,0.));
#13623=DIRECTION('',(0.,-1.,2.22044604925031E-16));
#13624=DIRECTION('',(1.,0.,0.));
#13625=DIRECTION('',(0.,-1.,2.22044604925031E-16));
#13626=DIRECTION('',(1.,0.,0.));
#13627=DIRECTION('',(0.,0.,1.));
#13628=DIRECTION('',(2.22044604925031E-16,-1.,0.));
#13629=DIRECTION('',(0.,0.,1.));
#13630=DIRECTION('',(2.22044604925031E-16,1.,0.));
#13631=DIRECTION('',(0.,0.,1.));
#13632=DIRECTION('',(2.22044604925031E-16,1.,0.));
#13633=DIRECTION('',(0.,0.,1.));
#13634=DIRECTION('',(2.22044604925031E-16,1.,0.));
#13635=DIRECTION('',(0.,0.,1.));
#13636=DIRECTION('',(2.22044604925031E-16,1.,0.));
#13637=DIRECTION('',(0.,0.,1.));
#13638=DIRECTION('',(2.22044604925031E-16,-1.,0.));
#13639=DIRECTION('',(0.,0.,1.));
#13640=DIRECTION('',(2.22044604925031E-16,-1.,0.));
#13641=DIRECTION('',(0.,0.,1.));
#13642=DIRECTION('',(2.22044604925031E-16,-1.,0.));
#13643=DIRECTION('',(0.,0.,1.));
#13644=DIRECTION('',(2.22044604925031E-16,-1.,0.));
#13645=DIRECTION('',(0.,0.,1.));
#13646=DIRECTION('',(1.,0.,0.));
#13647=DIRECTION('',(0.,0.,1.));
#13648=DIRECTION('',(1.,0.,0.));
#13649=DIRECTION('',(0.,0.,1.));
#13650=DIRECTION('',(1.,0.,0.));
#13651=DIRECTION('',(0.,0.,1.));
#13652=DIRECTION('',(1.,0.,0.));
#13653=DIRECTION('',(0.,0.,1.));
#13654=DIRECTION('',(1.,0.,0.));
#13655=DIRECTION('',(0.,0.,1.));
#13656=DIRECTION('',(1.,0.,0.));
#13657=DIRECTION('',(0.,0.,1.));
#13658=DIRECTION('',(1.,0.,0.));
#13659=DIRECTION('',(0.,-1.,2.22044604925031E-16));
#13660=DIRECTION('',(1.,0.,0.));
#13661=DIRECTION('',(0.,0.,1.));
#13662=DIRECTION('',(2.22044604925031E-16,1.,0.));
#13663=DIRECTION('',(0.,0.,1.));
#13664=DIRECTION('',(2.22044604925031E-16,-1.,0.));
#13665=DIRECTION('',(0.,-1.,2.22044604925031E-16));
#13666=DIRECTION('',(1.,0.,0.));
#13667=DIRECTION('',(0.,0.,1.));
#13668=DIRECTION('',(1.,0.,0.));
#13669=DIRECTION('',(0.,0.,1.));
#13670=DIRECTION('',(1.,0.,0.));
#13671=DIRECTION('',(0.,0.,1.));
#13672=DIRECTION('',(1.,0.,0.));
#13673=DIRECTION('',(0.,0.,1.));
#13674=DIRECTION('',(1.,0.,0.));
#13675=CARTESIAN_POINT('',(0.,0.,0.));
#13676=CARTESIAN_POINT('',(0.,0.,0.));
#13677=CARTESIAN_POINT('',(0.,0.,0.));
#13678=CARTESIAN_POINT('Origin',(11.5,-3.,-0.1));
#13679=CARTESIAN_POINT('',(11.335,-3.,0.));
#13680=CARTESIAN_POINT('Origin',(11.5,-3.,0.));
#13681=CARTESIAN_POINT('',(11.335,-3.,1.));
#13682=CARTESIAN_POINT('',(11.335,-3.,-0.1));
#13683=CARTESIAN_POINT('Origin',(11.5,-3.,1.));
#13684=CARTESIAN_POINT('Origin',(11.5,3.,-0.1));
#13685=CARTESIAN_POINT('',(11.335,3.,0.));
#13686=CARTESIAN_POINT('Origin',(11.5,3.,0.));
#13687=CARTESIAN_POINT('',(11.335,3.,1.));
#13688=CARTESIAN_POINT('',(11.335,3.,-0.1));
#13689=CARTESIAN_POINT('Origin',(11.5,3.,1.));
#13690=CARTESIAN_POINT('Origin',(-11.5,-3.,-0.1));
#13691=CARTESIAN_POINT('',(-11.665,-3.,0.));
#13692=CARTESIAN_POINT('Origin',(-11.5,-3.,0.));
#13693=CARTESIAN_POINT('',(-11.665,-3.,1.));
#13694=CARTESIAN_POINT('',(-11.665,-3.,-0.1));
#13695=CARTESIAN_POINT('Origin',(-11.5,-3.,1.));
#13696=CARTESIAN_POINT('Origin',(-11.5,3.,-0.1));
#13697=CARTESIAN_POINT('',(-11.665,3.,0.));
#13698=CARTESIAN_POINT('Origin',(-11.5,3.,0.));
#13699=CARTESIAN_POINT('',(-11.665,3.,1.));
#13700=CARTESIAN_POINT('',(-11.665,3.,-0.1));
#13701=CARTESIAN_POINT('Origin',(-11.5,3.,1.));
#13702=CARTESIAN_POINT('Origin',(13.5,1.9,-0.1));
#13703=CARTESIAN_POINT('',(13.335,1.9,0.));
#13704=CARTESIAN_POINT('Origin',(13.5,1.9,0.));
#13705=CARTESIAN_POINT('',(13.335,1.9,1.));
#13706=CARTESIAN_POINT('',(13.335,1.9,-0.1));
#13707=CARTESIAN_POINT('Origin',(13.5,1.9,1.));
#13708=CARTESIAN_POINT('Origin',(13.5,4.1,-0.1));
#13709=CARTESIAN_POINT('',(13.335,4.1,0.));
#13710=CARTESIAN_POINT('Origin',(13.5,4.1,0.));
#13711=CARTESIAN_POINT('',(13.335,4.1,1.));
#13712=CARTESIAN_POINT('',(13.335,4.1,-0.1));
#13713=CARTESIAN_POINT('Origin',(13.5,4.1,1.));
#13714=CARTESIAN_POINT('Origin',(-13.5,1.9,-0.1));
#13715=CARTESIAN_POINT('',(-13.665,1.9,0.));
#13716=CARTESIAN_POINT('Origin',(-13.5,1.9,0.));
#13717=CARTESIAN_POINT('',(-13.665,1.9,1.));
#13718=CARTESIAN_POINT('',(-13.665,1.9,-0.1));
#13719=CARTESIAN_POINT('Origin',(-13.5,1.9,1.));
#13720=CARTESIAN_POINT('Origin',(-13.5,4.1,-0.1));
#13721=CARTESIAN_POINT('',(-13.665,4.1,0.));
#13722=CARTESIAN_POINT('Origin',(-13.5,4.1,0.));
#13723=CARTESIAN_POINT('',(-13.665,4.1,1.));
#13724=CARTESIAN_POINT('',(-13.665,4.1,-0.1));
#13725=CARTESIAN_POINT('Origin',(-13.5,4.1,1.));
#13726=CARTESIAN_POINT('Origin',(13.5,-4.1,-0.1));
#13727=CARTESIAN_POINT('',(13.335,-4.1,0.));
#13728=CARTESIAN_POINT('Origin',(13.5,-4.1,0.));
#13729=CARTESIAN_POINT('',(13.335,-4.1,1.));
#13730=CARTESIAN_POINT('',(13.335,-4.1,-0.1));
#13731=CARTESIAN_POINT('Origin',(13.5,-4.1,1.));
#13732=CARTESIAN_POINT('Origin',(13.5,-1.9,-0.1));
#13733=CARTESIAN_POINT('',(13.335,-1.9,0.));
#13734=CARTESIAN_POINT('Origin',(13.5,-1.9,0.));
#13735=CARTESIAN_POINT('',(13.335,-1.9,1.));
#13736=CARTESIAN_POINT('',(13.335,-1.9,-0.1));
#13737=CARTESIAN_POINT('Origin',(13.5,-1.9,1.));
#13738=CARTESIAN_POINT('Origin',(-13.5,-4.1,-0.1));
#13739=CARTESIAN_POINT('',(-13.665,-4.1,0.));
#13740=CARTESIAN_POINT('Origin',(-13.5,-4.1,0.));
#13741=CARTESIAN_POINT('',(-13.665,-4.1,1.));
#13742=CARTESIAN_POINT('',(-13.665,-4.1,-0.1));
#13743=CARTESIAN_POINT('Origin',(-13.5,-4.1,1.));
#13744=CARTESIAN_POINT('Origin',(-13.5,-1.9,-0.1));
#13745=CARTESIAN_POINT('',(-13.665,-1.9,0.));
#13746=CARTESIAN_POINT('Origin',(-13.5,-1.9,0.));
#13747=CARTESIAN_POINT('',(-13.665,-1.9,1.));
#13748=CARTESIAN_POINT('',(-13.665,-1.9,-0.1));
#13749=CARTESIAN_POINT('Origin',(-13.5,-1.9,1.));
#13750=CARTESIAN_POINT('Origin',(16.,7.,0.));
#13751=CARTESIAN_POINT('',(16.,7.,0.));
#13752=CARTESIAN_POINT('',(-16.,7.,0.));
#13753=CARTESIAN_POINT('',(16.,7.,0.));
#13754=CARTESIAN_POINT('',(-16.,7.,1.));
#13755=CARTESIAN_POINT('',(-16.,7.,0.));
#13756=CARTESIAN_POINT('',(16.,7.,1.));
#13757=CARTESIAN_POINT('',(16.,7.,1.));
#13758=CARTESIAN_POINT('',(16.,7.,0.));
#13759=CARTESIAN_POINT('Origin',(16.,-7.,0.));
#13760=CARTESIAN_POINT('',(16.,-7.,0.));
#13761=CARTESIAN_POINT('',(16.,-7.,0.));
#13762=CARTESIAN_POINT('',(16.,-7.,1.));
#13763=CARTESIAN_POINT('',(16.,-7.,1.));
#13764=CARTESIAN_POINT('',(16.,-7.,0.));
#13765=CARTESIAN_POINT('Origin',(-16.,-7.,0.));
#13766=CARTESIAN_POINT('',(-16.,-7.,0.));
#13767=CARTESIAN_POINT('',(-16.,-7.,0.));
#13768=CARTESIAN_POINT('',(-16.,-7.,1.));
#13769=CARTESIAN_POINT('',(-16.,-7.,1.));
#13770=CARTESIAN_POINT('',(-16.,-7.,0.));
#13771=CARTESIAN_POINT('Origin',(-16.,7.,0.));
#13772=CARTESIAN_POINT('',(-16.,7.,0.));
#13773=CARTESIAN_POINT('',(-16.,7.,1.));
#13774=CARTESIAN_POINT('Origin',(0.,0.,1.));
#13775=CARTESIAN_POINT('Origin',(0.,0.,0.));
#13776=CARTESIAN_POINT('',(0.,0.,0.));
#13777=CARTESIAN_POINT('Origin',(-15.,7.,-0.8));
#13778=CARTESIAN_POINT('',(-15.,7.,-0.8));
#13779=CARTESIAN_POINT('',(-16.,7.,-0.8));
#13780=CARTESIAN_POINT('',(-15.,7.,-0.8));
#13781=CARTESIAN_POINT('',(-16.,7.,0.));
#13782=CARTESIAN_POINT('',(-16.,7.,-0.8));
#13783=CARTESIAN_POINT('',(-15.,7.,0.));
#13784=CARTESIAN_POINT('',(-15.,7.,0.));
#13785=CARTESIAN_POINT('',(-15.,7.,-0.8));
#13786=CARTESIAN_POINT('Origin',(-15.,-7.,-0.8));
#13787=CARTESIAN_POINT('',(-15.,-7.,-0.8));
#13788=CARTESIAN_POINT('',(-15.,-7.,-0.8));
#13789=CARTESIAN_POINT('',(-15.,-7.,0.));
#13790=CARTESIAN_POINT('',(-15.,-7.,0.));
#13791=CARTESIAN_POINT('',(-15.,-7.,-0.8));
#13792=CARTESIAN_POINT('Origin',(-16.,-7.,-0.8));
#13793=CARTESIAN_POINT('',(-16.,-7.,-0.8));
#13794=CARTESIAN_POINT('',(-16.,-7.,-0.8));
#13795=CARTESIAN_POINT('',(-16.,-7.,0.));
#13796=CARTESIAN_POINT('',(-16.,-7.,0.));
#13797=CARTESIAN_POINT('',(-16.,-7.,-0.8));
#13798=CARTESIAN_POINT('Origin',(-16.,7.,-0.8));
#13799=CARTESIAN_POINT('',(-16.,7.,-0.8));
#13800=CARTESIAN_POINT('',(-16.,7.,0.));
#13801=CARTESIAN_POINT('Origin',(-15.5,0.,0.));
#13802=CARTESIAN_POINT('Origin',(-15.5,0.,-0.8));
#13803=CARTESIAN_POINT('',(0.,0.,0.));
#13804=CARTESIAN_POINT('Origin',(16.,7.,-0.8));
#13805=CARTESIAN_POINT('',(16.,7.,-0.8));
#13806=CARTESIAN_POINT('',(15.,7.,-0.8));
#13807=CARTESIAN_POINT('',(16.,7.,-0.8));
#13808=CARTESIAN_POINT('',(15.,7.,0.));
#13809=CARTESIAN_POINT('',(15.,7.,-0.8));
#13810=CARTESIAN_POINT('',(16.,7.,0.));
#13811=CARTESIAN_POINT('',(16.,7.,0.));
#13812=CARTESIAN_POINT('',(16.,7.,-0.8));
#13813=CARTESIAN_POINT('Origin',(16.,-7.,-0.8));
#13814=CARTESIAN_POINT('',(16.,-7.,-0.8));
#13815=CARTESIAN_POINT('',(16.,-7.,-0.8));
#13816=CARTESIAN_POINT('',(16.,-7.,0.));
#13817=CARTESIAN_POINT('',(16.,-7.,0.));
#13818=CARTESIAN_POINT('',(16.,-7.,-0.8));
#13819=CARTESIAN_POINT('Origin',(15.,-7.,-0.8));
#13820=CARTESIAN_POINT('',(15.,-7.,-0.8));
#13821=CARTESIAN_POINT('',(15.,-7.,-0.8));
#13822=CARTESIAN_POINT('',(15.,-7.,0.));
#13823=CARTESIAN_POINT('',(15.,-7.,0.));
#13824=CARTESIAN_POINT('',(15.,-7.,-0.8));
#13825=CARTESIAN_POINT('Origin',(15.,7.,-0.8));
#13826=CARTESIAN_POINT('',(15.,7.,-0.8));
#13827=CARTESIAN_POINT('',(15.,7.,0.));
#13828=CARTESIAN_POINT('Origin',(15.5,0.,0.));
#13829=CARTESIAN_POINT('Origin',(15.5,0.,-0.8));
#13830=CARTESIAN_POINT('',(0.,0.,0.));
#13831=CARTESIAN_POINT('Origin',(-13.5,-1.9,2.));
#13832=CARTESIAN_POINT('',(-13.9,-1.9,2.));
#13833=CARTESIAN_POINT('',(-13.9,-1.9,5.));
#13834=CARTESIAN_POINT('',(-13.9,-1.9,2.));
#13835=CARTESIAN_POINT('',(-13.5,-1.5,2.));
#13836=CARTESIAN_POINT('Origin',(-13.5,-1.9,2.));
#13837=CARTESIAN_POINT('',(-13.5,-1.5,5.));
#13838=CARTESIAN_POINT('',(-13.5,-1.5,2.));
#13839=CARTESIAN_POINT('Origin',(-13.5,-1.9,5.));
#13840=CARTESIAN_POINT('Origin',(-13.5,-4.1,2.));
#13841=CARTESIAN_POINT('',(-13.9,-4.1,2.));
#13842=CARTESIAN_POINT('',(-13.9,-4.1,5.));
#13843=CARTESIAN_POINT('',(-13.9,-4.1,2.));
#13844=CARTESIAN_POINT('',(-13.5,-4.5,2.));
#13845=CARTESIAN_POINT('Origin',(-13.5,-4.1,2.));
#13846=CARTESIAN_POINT('',(-13.5,-4.5,5.));
#13847=CARTESIAN_POINT('',(-13.5,-4.5,2.));
#13848=CARTESIAN_POINT('Origin',(-13.5,-4.1,5.));
#13849=CARTESIAN_POINT('Origin',(-13.5,-3.,4.59));
#13850=CARTESIAN_POINT('',(-13.6237941840314,-3.10908712114636,4.59));
#13851=CARTESIAN_POINT('',(-13.3762058159686,-3.10908712114636,4.59));
#13852=CARTESIAN_POINT('',(-14.1,-3.10908712114636,4.59));
#13853=CARTESIAN_POINT('Origin',(-13.5,-3.,4.59));
#13854=CARTESIAN_POINT('Origin',(-13.5,-3.,4.59));
#13855=CARTESIAN_POINT('',(-13.6237941840314,-2.89091287885364,4.59));
#13856=CARTESIAN_POINT('',(-13.665,-3.,4.6));
#13857=CARTESIAN_POINT('Ctrl Pts',(-13.6237941840314,-2.89091287885364,
4.59));
#13858=CARTESIAN_POINT('Ctrl Pts',(-13.6353991351895,-2.90408240284739,
4.59243495840567));
#13859=CARTESIAN_POINT('Ctrl Pts',(-13.6453456436582,-2.91977655056228,
4.59485638705045));
#13860=CARTESIAN_POINT('Ctrl Pts',(-13.660814864634,-2.95701983403981,4.59880705606552));
#13861=CARTESIAN_POINT('Ctrl Pts',(-13.665,-2.97916814649112,4.6));
#13862=CARTESIAN_POINT('Ctrl Pts',(-13.665,-3.,4.6));
#13863=CARTESIAN_POINT('',(-13.3762058159686,-2.89091287885364,4.59));
#13864=CARTESIAN_POINT('Origin',(-13.5,-3.,4.59));
#13865=CARTESIAN_POINT('',(-13.335,-3.,4.6));
#13866=CARTESIAN_POINT('Ctrl Pts',(-13.335,-3.,4.6));
#13867=CARTESIAN_POINT('Ctrl Pts',(-13.335,-2.97916814649112,4.6));
#13868=CARTESIAN_POINT('Ctrl Pts',(-13.339185135366,-2.95701983403981,4.59880705606552));
#13869=CARTESIAN_POINT('Ctrl Pts',(-13.3546543563418,-2.91977655056228,
4.59485638705045));
#13870=CARTESIAN_POINT('Ctrl Pts',(-13.3646008648105,-2.90408240284739,
4.59243495840567));
#13871=CARTESIAN_POINT('Ctrl Pts',(-13.3762058159686,-2.89091287885364,
4.59));
#13872=CARTESIAN_POINT('Ctrl Pts',(-13.3762058159686,-3.10908712114636,
4.59));
#13873=CARTESIAN_POINT('Ctrl Pts',(-13.3646008648105,-3.09591759715261,
4.59243495840567));
#13874=CARTESIAN_POINT('Ctrl Pts',(-13.3546543563418,-3.08022344943772,
4.59485638705045));
#13875=CARTESIAN_POINT('Ctrl Pts',(-13.339185135366,-3.04298016596019,4.59880705606552));
#13876=CARTESIAN_POINT('Ctrl Pts',(-13.335,-3.02083185350888,4.6));
#13877=CARTESIAN_POINT('Ctrl Pts',(-13.335,-3.,4.6));
#13878=CARTESIAN_POINT('Ctrl Pts',(-13.665,-3.,4.6));
#13879=CARTESIAN_POINT('Ctrl Pts',(-13.665,-3.02083185350888,4.6));
#13880=CARTESIAN_POINT('Ctrl Pts',(-13.660814864634,-3.04298016596019,4.59880705606552));
#13881=CARTESIAN_POINT('Ctrl Pts',(-13.6453456436582,-3.08022344943772,
4.59485638705045));
#13882=CARTESIAN_POINT('Ctrl Pts',(-13.6353991351895,-3.09591759715261,
4.59243495840567));
#13883=CARTESIAN_POINT('Ctrl Pts',(-13.6237941840314,-3.10908712114636,
4.59));
#13884=CARTESIAN_POINT('',(-13.665,-3.,5.));
#13885=CARTESIAN_POINT('',(-13.665,-3.,4.59));
#13886=CARTESIAN_POINT('Origin',(-13.5,-3.,5.));
#13887=CARTESIAN_POINT('Origin',(-13.5,-3.,4.59));
#13888=CARTESIAN_POINT('',(-14.1,-2.89091287885364,4.59));
#13889=CARTESIAN_POINT('Origin',(-13.5,-4.1,2.));
#13890=CARTESIAN_POINT('Origin',(-13.5,-4.1,5.));
#13891=CARTESIAN_POINT('',(-13.5,-4.5,2.));
#13892=CARTESIAN_POINT('Origin',(-13.5,-4.1,2.));
#13893=CARTESIAN_POINT('Origin',(-13.5,-4.1,2.));
#13894=CARTESIAN_POINT('',(-13.725,-4.1,2.));
#13895=CARTESIAN_POINT('Origin',(-13.5,-4.1,2.));
#13896=CARTESIAN_POINT('Origin',(-13.5,-1.9,2.));
#13897=CARTESIAN_POINT('Origin',(-13.5,-1.9,5.));
#13898=CARTESIAN_POINT('',(-13.5,-1.5,2.));
#13899=CARTESIAN_POINT('Origin',(-13.5,-1.9,2.));
#13900=CARTESIAN_POINT('Origin',(-13.5,-1.9,2.));
#13901=CARTESIAN_POINT('',(-13.725,-1.9,2.));
#13902=CARTESIAN_POINT('Origin',(-13.5,-1.9,2.));
#13903=CARTESIAN_POINT('Origin',(-13.5,-3.,5.));
#13904=CARTESIAN_POINT('',(-14.,-1.5,5.));
#13905=CARTESIAN_POINT('',(-14.,-4.5,5.));
#13906=CARTESIAN_POINT('',(-14.,-1.5,5.));
#13907=CARTESIAN_POINT('',(-14.,-4.5,5.));
#13908=CARTESIAN_POINT('',(-13.,-4.5,5.));
#13909=CARTESIAN_POINT('',(-14.,-4.5,5.));
#13910=CARTESIAN_POINT('',(-13.,-1.5,5.));
#13911=CARTESIAN_POINT('',(-13.,-4.5,5.));
#13912=CARTESIAN_POINT('',(-13.,-1.5,5.));
#13913=CARTESIAN_POINT('',(-13.,-1.5,5.));
#13914=CARTESIAN_POINT('Origin',(-13.5,-4.1,0.9));
#13915=CARTESIAN_POINT('',(-13.725,-4.1,1.));
#13916=CARTESIAN_POINT('Origin',(-13.5,-4.1,1.));
#13917=CARTESIAN_POINT('',(-13.725,-4.1,0.9));
#13918=CARTESIAN_POINT('Origin',(-13.5,-1.9,0.9));
#13919=CARTESIAN_POINT('',(-13.725,-1.9,1.));
#13920=CARTESIAN_POINT('Origin',(-13.5,-1.9,1.));
#13921=CARTESIAN_POINT('',(-13.725,-1.9,0.9));
#13922=CARTESIAN_POINT('Origin',(-14.1,-3.,4.));
#13923=CARTESIAN_POINT('',(-14.,-3.,4.6));
#13924=CARTESIAN_POINT('Origin',(-14.,-3.,4.));
#13925=CARTESIAN_POINT('',(-14.1,-3.,4.6));
#13926=CARTESIAN_POINT('',(-13.,-3.,4.6));
#13927=CARTESIAN_POINT('',(-14.1,-3.,4.6));
#13928=CARTESIAN_POINT('Origin',(-13.,-3.,4.));
#13929=CARTESIAN_POINT('Origin',(-13.,-1.5,1.));
#13930=CARTESIAN_POINT('',(-13.,-1.5,1.));
#13931=CARTESIAN_POINT('',(-14.,-1.5,1.));
#13932=CARTESIAN_POINT('',(-13.,-1.5,1.));
#13933=CARTESIAN_POINT('',(-14.,-1.5,1.));
#13934=CARTESIAN_POINT('',(-13.,-1.5,1.));
#13935=CARTESIAN_POINT('Origin',(-13.,-4.5,1.));
#13936=CARTESIAN_POINT('',(-13.,-4.5,1.));
#13937=CARTESIAN_POINT('',(-13.,-4.5,1.));
#13938=CARTESIAN_POINT('',(-13.,-4.5,1.));
#13939=CARTESIAN_POINT('Origin',(-14.,-4.5,1.));
#13940=CARTESIAN_POINT('',(-14.,-4.5,1.));
#13941=CARTESIAN_POINT('',(-14.,-4.5,1.));
#13942=CARTESIAN_POINT('',(-14.,-4.5,1.));
#13943=CARTESIAN_POINT('Origin',(-14.,-1.5,1.));
#13944=CARTESIAN_POINT('',(-14.,-1.5,1.));
#13945=CARTESIAN_POINT('Origin',(-13.5,-3.,1.));
#13946=CARTESIAN_POINT('',(0.,0.,0.));
#13947=CARTESIAN_POINT('Origin',(13.5,-1.9,2.));
#13948=CARTESIAN_POINT('',(13.1,-1.9,2.));
#13949=CARTESIAN_POINT('',(13.1,-1.9,5.));
#13950=CARTESIAN_POINT('',(13.1,-1.9,2.));
#13951=CARTESIAN_POINT('',(13.5,-1.5,2.));
#13952=CARTESIAN_POINT('Origin',(13.5,-1.9,2.));
#13953=CARTESIAN_POINT('',(13.5,-1.5,5.));
#13954=CARTESIAN_POINT('',(13.5,-1.5,2.));
#13955=CARTESIAN_POINT('Origin',(13.5,-1.9,5.));
#13956=CARTESIAN_POINT('Origin',(13.5,-4.1,2.));
#13957=CARTESIAN_POINT('',(13.1,-4.1,2.));
#13958=CARTESIAN_POINT('',(13.1,-4.1,5.));
#13959=CARTESIAN_POINT('',(13.1,-4.1,2.));
#13960=CARTESIAN_POINT('',(13.5,-4.5,2.));
#13961=CARTESIAN_POINT('Origin',(13.5,-4.1,2.));
#13962=CARTESIAN_POINT('',(13.5,-4.5,5.));
#13963=CARTESIAN_POINT('',(13.5,-4.5,2.));
#13964=CARTESIAN_POINT('Origin',(13.5,-4.1,5.));
#13965=CARTESIAN_POINT('Origin',(13.5,-3.,4.59));
#13966=CARTESIAN_POINT('',(13.3762058159686,-3.10908712114636,4.59));
#13967=CARTESIAN_POINT('',(13.6237941840314,-3.10908712114636,4.59));
#13968=CARTESIAN_POINT('',(12.9,-3.10908712114636,4.59));
#13969=CARTESIAN_POINT('Origin',(13.5,-3.,4.59));
#13970=CARTESIAN_POINT('Origin',(13.5,-3.,4.59));
#13971=CARTESIAN_POINT('',(13.3762058159686,-2.89091287885364,4.59));
#13972=CARTESIAN_POINT('',(13.335,-3.,4.6));
#13973=CARTESIAN_POINT('Ctrl Pts',(13.3762058159686,-2.89091287885364,4.59));
#13974=CARTESIAN_POINT('Ctrl Pts',(13.3646008648105,-2.90408240284739,4.59243495840567));
#13975=CARTESIAN_POINT('Ctrl Pts',(13.3546543563418,-2.91977655056228,4.59485638705045));
#13976=CARTESIAN_POINT('Ctrl Pts',(13.339185135366,-2.95701983403981,4.59880705606552));
#13977=CARTESIAN_POINT('Ctrl Pts',(13.335,-2.97916814649112,4.6));
#13978=CARTESIAN_POINT('Ctrl Pts',(13.335,-3.,4.6));
#13979=CARTESIAN_POINT('',(13.6237941840314,-2.89091287885364,4.59));
#13980=CARTESIAN_POINT('Origin',(13.5,-3.,4.59));
#13981=CARTESIAN_POINT('',(13.665,-3.,4.6));
#13982=CARTESIAN_POINT('Ctrl Pts',(13.665,-3.,4.6));
#13983=CARTESIAN_POINT('Ctrl Pts',(13.665,-2.97916814649112,4.6));
#13984=CARTESIAN_POINT('Ctrl Pts',(13.660814864634,-2.95701983403981,4.59880705606552));
#13985=CARTESIAN_POINT('Ctrl Pts',(13.6453456436582,-2.91977655056228,4.59485638705045));
#13986=CARTESIAN_POINT('Ctrl Pts',(13.6353991351895,-2.90408240284739,4.59243495840567));
#13987=CARTESIAN_POINT('Ctrl Pts',(13.6237941840314,-2.89091287885364,4.59));
#13988=CARTESIAN_POINT('Ctrl Pts',(13.6237941840314,-3.10908712114636,4.59));
#13989=CARTESIAN_POINT('Ctrl Pts',(13.6353991351895,-3.09591759715261,4.59243495840567));
#13990=CARTESIAN_POINT('Ctrl Pts',(13.6453456436582,-3.08022344943772,4.59485638705045));
#13991=CARTESIAN_POINT('Ctrl Pts',(13.660814864634,-3.04298016596019,4.59880705606552));
#13992=CARTESIAN_POINT('Ctrl Pts',(13.665,-3.02083185350888,4.6));
#13993=CARTESIAN_POINT('Ctrl Pts',(13.665,-3.,4.6));
#13994=CARTESIAN_POINT('Ctrl Pts',(13.335,-3.,4.6));
#13995=CARTESIAN_POINT('Ctrl Pts',(13.335,-3.02083185350888,4.6));
#13996=CARTESIAN_POINT('Ctrl Pts',(13.339185135366,-3.04298016596019,4.59880705606552));
#13997=CARTESIAN_POINT('Ctrl Pts',(13.3546543563418,-3.08022344943772,4.59485638705045));
#13998=CARTESIAN_POINT('Ctrl Pts',(13.3646008648105,-3.09591759715261,4.59243495840567));
#13999=CARTESIAN_POINT('Ctrl Pts',(13.3762058159686,-3.10908712114636,4.59));
#14000=CARTESIAN_POINT('',(13.335,-3.,5.));
#14001=CARTESIAN_POINT('',(13.335,-3.,4.59));
#14002=CARTESIAN_POINT('Origin',(13.5,-3.,5.));
#14003=CARTESIAN_POINT('Origin',(13.5,-3.,4.59));
#14004=CARTESIAN_POINT('',(12.9,-2.89091287885364,4.59));
#14005=CARTESIAN_POINT('Origin',(13.5,-4.1,2.));
#14006=CARTESIAN_POINT('Origin',(13.5,-4.1,5.));
#14007=CARTESIAN_POINT('',(13.5,-4.5,2.));
#14008=CARTESIAN_POINT('Origin',(13.5,-4.1,2.));
#14009=CARTESIAN_POINT('Origin',(13.5,-4.1,2.));
#14010=CARTESIAN_POINT('',(13.275,-4.1,2.));
#14011=CARTESIAN_POINT('Origin',(13.5,-4.1,2.));
#14012=CARTESIAN_POINT('Origin',(13.5,-1.9,2.));
#14013=CARTESIAN_POINT('Origin',(13.5,-1.9,5.));
#14014=CARTESIAN_POINT('',(13.5,-1.5,2.));
#14015=CARTESIAN_POINT('Origin',(13.5,-1.9,2.));
#14016=CARTESIAN_POINT('Origin',(13.5,-1.9,2.));
#14017=CARTESIAN_POINT('',(13.275,-1.9,2.));
#14018=CARTESIAN_POINT('Origin',(13.5,-1.9,2.));
#14019=CARTESIAN_POINT('Origin',(13.5,-3.,5.));
#14020=CARTESIAN_POINT('',(13.,-1.5,5.));
#14021=CARTESIAN_POINT('',(13.,-4.5,5.));
#14022=CARTESIAN_POINT('',(13.,-1.5,5.));
#14023=CARTESIAN_POINT('',(13.,-4.5,5.));
#14024=CARTESIAN_POINT('',(14.,-4.5,5.));
#14025=CARTESIAN_POINT('',(13.,-4.5,5.));
#14026=CARTESIAN_POINT('',(14.,-1.5,5.));
#14027=CARTESIAN_POINT('',(14.,-4.5,5.));
#14028=CARTESIAN_POINT('',(14.,-1.5,5.));
#14029=CARTESIAN_POINT('',(14.,-1.5,5.));
#14030=CARTESIAN_POINT('Origin',(13.5,-4.1,0.9));
#14031=CARTESIAN_POINT('',(13.275,-4.1,1.));
#14032=CARTESIAN_POINT('Origin',(13.5,-4.1,1.));
#14033=CARTESIAN_POINT('',(13.275,-4.1,0.9));
#14034=CARTESIAN_POINT('Origin',(13.5,-1.9,0.9));
#14035=CARTESIAN_POINT('',(13.275,-1.9,1.));
#14036=CARTESIAN_POINT('Origin',(13.5,-1.9,1.));
#14037=CARTESIAN_POINT('',(13.275,-1.9,0.9));
#14038=CARTESIAN_POINT('Origin',(12.9,-3.,4.));
#14039=CARTESIAN_POINT('',(13.,-3.,4.6));
#14040=CARTESIAN_POINT('Origin',(13.,-3.,4.));
#14041=CARTESIAN_POINT('',(12.9,-3.,4.6));
#14042=CARTESIAN_POINT('',(14.,-3.,4.6));
#14043=CARTESIAN_POINT('',(12.9,-3.,4.6));
#14044=CARTESIAN_POINT('Origin',(14.,-3.,4.));
#14045=CARTESIAN_POINT('Origin',(14.,-1.5,1.));
#14046=CARTESIAN_POINT('',(14.,-1.5,1.));
#14047=CARTESIAN_POINT('',(13.,-1.5,1.));
#14048=CARTESIAN_POINT('',(14.,-1.5,1.));
#14049=CARTESIAN_POINT('',(13.,-1.5,1.));
#14050=CARTESIAN_POINT('',(14.,-1.5,1.));
#14051=CARTESIAN_POINT('Origin',(14.,-4.5,1.));
#14052=CARTESIAN_POINT('',(14.,-4.5,1.));
#14053=CARTESIAN_POINT('',(14.,-4.5,1.));
#14054=CARTESIAN_POINT('',(14.,-4.5,1.));
#14055=CARTESIAN_POINT('Origin',(13.,-4.5,1.));
#14056=CARTESIAN_POINT('',(13.,-4.5,1.));
#14057=CARTESIAN_POINT('',(13.,-4.5,1.));
#14058=CARTESIAN_POINT('',(13.,-4.5,1.));
#14059=CARTESIAN_POINT('Origin',(13.,-1.5,1.));
#14060=CARTESIAN_POINT('',(13.,-1.5,1.));
#14061=CARTESIAN_POINT('Origin',(13.5,-3.,1.));
#14062=CARTESIAN_POINT('',(0.,0.,0.));
#14063=CARTESIAN_POINT('Origin',(-13.5,4.1,2.));
#14064=CARTESIAN_POINT('',(-13.9,4.1,2.));
#14065=CARTESIAN_POINT('',(-13.9,4.1,5.));
#14066=CARTESIAN_POINT('',(-13.9,4.1,2.));
#14067=CARTESIAN_POINT('',(-13.5,4.5,2.));
#14068=CARTESIAN_POINT('Origin',(-13.5,4.1,2.));
#14069=CARTESIAN_POINT('',(-13.5,4.5,5.));
#14070=CARTESIAN_POINT('',(-13.5,4.5,2.));
#14071=CARTESIAN_POINT('Origin',(-13.5,4.1,5.));
#14072=CARTESIAN_POINT('Origin',(-13.5,1.9,2.));
#14073=CARTESIAN_POINT('',(-13.9,1.9,2.));
#14074=CARTESIAN_POINT('',(-13.9,1.9,5.));
#14075=CARTESIAN_POINT('',(-13.9,1.9,2.));
#14076=CARTESIAN_POINT('',(-13.5,1.5,2.));
#14077=CARTESIAN_POINT('Origin',(-13.5,1.9,2.));
#14078=CARTESIAN_POINT('',(-13.5,1.5,5.));
#14079=CARTESIAN_POINT('',(-13.5,1.5,2.));
#14080=CARTESIAN_POINT('Origin',(-13.5,1.9,5.));
#14081=CARTESIAN_POINT('Origin',(-13.5,3.,4.59));
#14082=CARTESIAN_POINT('',(-13.6237941840314,2.89091287885364,4.59));
#14083=CARTESIAN_POINT('',(-13.3762058159686,2.89091287885364,4.59));
#14084=CARTESIAN_POINT('',(-14.1,2.89091287885364,4.59));
#14085=CARTESIAN_POINT('Origin',(-13.5,3.,4.59));
#14086=CARTESIAN_POINT('Origin',(-13.5,3.,4.59));
#14087=CARTESIAN_POINT('',(-13.6237941840314,3.10908712114636,4.59));
#14088=CARTESIAN_POINT('',(-13.665,3.,4.6));
#14089=CARTESIAN_POINT('Ctrl Pts',(-13.6237941840314,3.10908712114636,4.59));
#14090=CARTESIAN_POINT('Ctrl Pts',(-13.6353991351895,3.09591759715261,4.59243495840567));
#14091=CARTESIAN_POINT('Ctrl Pts',(-13.6453456436582,3.08022344943772,4.59485638705045));
#14092=CARTESIAN_POINT('Ctrl Pts',(-13.660814864634,3.04298016596019,4.59880705606552));
#14093=CARTESIAN_POINT('Ctrl Pts',(-13.665,3.02083185350888,4.6));
#14094=CARTESIAN_POINT('Ctrl Pts',(-13.665,3.,4.6));
#14095=CARTESIAN_POINT('',(-13.3762058159686,3.10908712114636,4.59));
#14096=CARTESIAN_POINT('Origin',(-13.5,3.,4.59));
#14097=CARTESIAN_POINT('',(-13.335,3.,4.6));
#14098=CARTESIAN_POINT('Ctrl Pts',(-13.335,3.,4.6));
#14099=CARTESIAN_POINT('Ctrl Pts',(-13.335,3.02083185350888,4.6));
#14100=CARTESIAN_POINT('Ctrl Pts',(-13.339185135366,3.04298016596019,4.59880705606552));
#14101=CARTESIAN_POINT('Ctrl Pts',(-13.3546543563418,3.08022344943772,4.59485638705045));
#14102=CARTESIAN_POINT('Ctrl Pts',(-13.3646008648105,3.09591759715261,4.59243495840567));
#14103=CARTESIAN_POINT('Ctrl Pts',(-13.3762058159686,3.10908712114636,4.59));
#14104=CARTESIAN_POINT('Ctrl Pts',(-13.3762058159686,2.89091287885364,4.59));
#14105=CARTESIAN_POINT('Ctrl Pts',(-13.3646008648105,2.90408240284739,4.59243495840567));
#14106=CARTESIAN_POINT('Ctrl Pts',(-13.3546543563418,2.91977655056228,4.59485638705045));
#14107=CARTESIAN_POINT('Ctrl Pts',(-13.339185135366,2.95701983403981,4.59880705606552));
#14108=CARTESIAN_POINT('Ctrl Pts',(-13.335,2.97916814649112,4.6));
#14109=CARTESIAN_POINT('Ctrl Pts',(-13.335,3.,4.6));
#14110=CARTESIAN_POINT('Ctrl Pts',(-13.665,3.,4.6));
#14111=CARTESIAN_POINT('Ctrl Pts',(-13.665,2.97916814649112,4.6));
#14112=CARTESIAN_POINT('Ctrl Pts',(-13.660814864634,2.95701983403981,4.59880705606552));
#14113=CARTESIAN_POINT('Ctrl Pts',(-13.6453456436582,2.91977655056228,4.59485638705045));
#14114=CARTESIAN_POINT('Ctrl Pts',(-13.6353991351895,2.90408240284739,4.59243495840567));
#14115=CARTESIAN_POINT('Ctrl Pts',(-13.6237941840314,2.89091287885364,4.59));
#14116=CARTESIAN_POINT('',(-13.665,3.,5.));
#14117=CARTESIAN_POINT('',(-13.665,3.,4.59));
#14118=CARTESIAN_POINT('Origin',(-13.5,3.,5.));
#14119=CARTESIAN_POINT('Origin',(-13.5,3.,4.59));
#14120=CARTESIAN_POINT('',(-14.1,3.10908712114636,4.59));
#14121=CARTESIAN_POINT('Origin',(-13.5,1.9,2.));
#14122=CARTESIAN_POINT('Origin',(-13.5,1.9,5.));
#14123=CARTESIAN_POINT('',(-13.5,1.5,2.));
#14124=CARTESIAN_POINT('Origin',(-13.5,1.9,2.));
#14125=CARTESIAN_POINT('Origin',(-13.5,1.9,2.));
#14126=CARTESIAN_POINT('',(-13.725,1.9,2.));
#14127=CARTESIAN_POINT('Origin',(-13.5,1.9,2.));
#14128=CARTESIAN_POINT('Origin',(-13.5,4.1,2.));
#14129=CARTESIAN_POINT('Origin',(-13.5,4.1,5.));
#14130=CARTESIAN_POINT('',(-13.5,4.5,2.));
#14131=CARTESIAN_POINT('Origin',(-13.5,4.1,2.));
#14132=CARTESIAN_POINT('Origin',(-13.5,4.1,2.));
#14133=CARTESIAN_POINT('',(-13.725,4.1,2.));
#14134=CARTESIAN_POINT('Origin',(-13.5,4.1,2.));
#14135=CARTESIAN_POINT('Origin',(-13.5,3.,5.));
#14136=CARTESIAN_POINT('',(-14.,4.5,5.));
#14137=CARTESIAN_POINT('',(-14.,1.5,5.));
#14138=CARTESIAN_POINT('',(-14.,4.5,5.));
#14139=CARTESIAN_POINT('',(-14.,1.5,5.));
#14140=CARTESIAN_POINT('',(-13.,1.5,5.));
#14141=CARTESIAN_POINT('',(-14.,1.5,5.));
#14142=CARTESIAN_POINT('',(-13.,4.5,5.));
#14143=CARTESIAN_POINT('',(-13.,1.5,5.));
#14144=CARTESIAN_POINT('',(-13.,4.5,5.));
#14145=CARTESIAN_POINT('',(-13.,4.5,5.));
#14146=CARTESIAN_POINT('Origin',(-13.5,1.9,0.9));
#14147=CARTESIAN_POINT('',(-13.725,1.9,1.));
#14148=CARTESIAN_POINT('Origin',(-13.5,1.9,1.));
#14149=CARTESIAN_POINT('',(-13.725,1.9,0.9));
#14150=CARTESIAN_POINT('Origin',(-13.5,4.1,0.9));
#14151=CARTESIAN_POINT('',(-13.725,4.1,1.));
#14152=CARTESIAN_POINT('Origin',(-13.5,4.1,1.));
#14153=CARTESIAN_POINT('',(-13.725,4.1,0.9));
#14154=CARTESIAN_POINT('Origin',(-14.1,3.,4.));
#14155=CARTESIAN_POINT('',(-14.,3.,4.6));
#14156=CARTESIAN_POINT('Origin',(-14.,3.,4.));
#14157=CARTESIAN_POINT('',(-14.1,3.,4.6));
#14158=CARTESIAN_POINT('',(-13.,3.,4.6));
#14159=CARTESIAN_POINT('',(-14.1,3.,4.6));
#14160=CARTESIAN_POINT('Origin',(-13.,3.,4.));
#14161=CARTESIAN_POINT('Origin',(-13.,4.5,1.));
#14162=CARTESIAN_POINT('',(-13.,4.5,1.));
#14163=CARTESIAN_POINT('',(-14.,4.5,1.));
#14164=CARTESIAN_POINT('',(-13.,4.5,1.));
#14165=CARTESIAN_POINT('',(-14.,4.5,1.));
#14166=CARTESIAN_POINT('',(-13.,4.5,1.));
#14167=CARTESIAN_POINT('Origin',(-13.,1.5,1.));
#14168=CARTESIAN_POINT('',(-13.,1.5,1.));
#14169=CARTESIAN_POINT('',(-13.,1.5,1.));
#14170=CARTESIAN_POINT('',(-13.,1.5,1.));
#14171=CARTESIAN_POINT('Origin',(-14.,1.5,1.));
#14172=CARTESIAN_POINT('',(-14.,1.5,1.));
#14173=CARTESIAN_POINT('',(-14.,1.5,1.));
#14174=CARTESIAN_POINT('',(-14.,1.5,1.));
#14175=CARTESIAN_POINT('Origin',(-14.,4.5,1.));
#14176=CARTESIAN_POINT('',(-14.,4.5,1.));
#14177=CARTESIAN_POINT('Origin',(-13.5,3.,1.));
#14178=CARTESIAN_POINT('',(0.,0.,0.));
#14179=CARTESIAN_POINT('Origin',(13.5,4.1,2.));
#14180=CARTESIAN_POINT('',(13.1,4.1,2.));
#14181=CARTESIAN_POINT('',(13.1,4.1,5.));
#14182=CARTESIAN_POINT('',(13.1,4.1,2.));
#14183=CARTESIAN_POINT('',(13.5,4.5,2.));
#14184=CARTESIAN_POINT('Origin',(13.5,4.1,2.));
#14185=CARTESIAN_POINT('',(13.5,4.5,5.));
#14186=CARTESIAN_POINT('',(13.5,4.5,2.));
#14187=CARTESIAN_POINT('Origin',(13.5,4.1,5.));
#14188=CARTESIAN_POINT('Origin',(13.5,1.9,2.));
#14189=CARTESIAN_POINT('',(13.1,1.9,2.));
#14190=CARTESIAN_POINT('',(13.1,1.9,5.));
#14191=CARTESIAN_POINT('',(13.1,1.9,2.));
#14192=CARTESIAN_POINT('',(13.5,1.5,2.));
#14193=CARTESIAN_POINT('Origin',(13.5,1.9,2.));
#14194=CARTESIAN_POINT('',(13.5,1.5,5.));
#14195=CARTESIAN_POINT('',(13.5,1.5,2.));
#14196=CARTESIAN_POINT('Origin',(13.5,1.9,5.));
#14197=CARTESIAN_POINT('Origin',(13.5,3.,4.59));
#14198=CARTESIAN_POINT('',(13.3762058159686,2.89091287885364,4.59));
#14199=CARTESIAN_POINT('',(13.6237941840314,2.89091287885364,4.59));
#14200=CARTESIAN_POINT('',(12.9,2.89091287885364,4.59));
#14201=CARTESIAN_POINT('Origin',(13.5,3.,4.59));
#14202=CARTESIAN_POINT('Origin',(13.5,3.,4.59));
#14203=CARTESIAN_POINT('',(13.3762058159686,3.10908712114636,4.59));
#14204=CARTESIAN_POINT('',(13.335,3.,4.6));
#14205=CARTESIAN_POINT('Ctrl Pts',(13.3762058159686,3.10908712114636,4.59));
#14206=CARTESIAN_POINT('Ctrl Pts',(13.3646008648105,3.09591759715261,4.59243495840567));
#14207=CARTESIAN_POINT('Ctrl Pts',(13.3546543563418,3.08022344943772,4.59485638705045));
#14208=CARTESIAN_POINT('Ctrl Pts',(13.339185135366,3.04298016596019,4.59880705606552));
#14209=CARTESIAN_POINT('Ctrl Pts',(13.335,3.02083185350888,4.6));
#14210=CARTESIAN_POINT('Ctrl Pts',(13.335,3.,4.6));
#14211=CARTESIAN_POINT('',(13.6237941840314,3.10908712114636,4.59));
#14212=CARTESIAN_POINT('Origin',(13.5,3.,4.59));
#14213=CARTESIAN_POINT('',(13.665,3.,4.6));
#14214=CARTESIAN_POINT('Ctrl Pts',(13.665,3.,4.6));
#14215=CARTESIAN_POINT('Ctrl Pts',(13.665,3.02083185350888,4.6));
#14216=CARTESIAN_POINT('Ctrl Pts',(13.660814864634,3.04298016596019,4.59880705606552));
#14217=CARTESIAN_POINT('Ctrl Pts',(13.6453456436582,3.08022344943772,4.59485638705045));
#14218=CARTESIAN_POINT('Ctrl Pts',(13.6353991351895,3.09591759715261,4.59243495840567));
#14219=CARTESIAN_POINT('Ctrl Pts',(13.6237941840314,3.10908712114636,4.59));
#14220=CARTESIAN_POINT('Ctrl Pts',(13.6237941840314,2.89091287885364,4.59));
#14221=CARTESIAN_POINT('Ctrl Pts',(13.6353991351895,2.90408240284739,4.59243495840567));
#14222=CARTESIAN_POINT('Ctrl Pts',(13.6453456436582,2.91977655056228,4.59485638705045));
#14223=CARTESIAN_POINT('Ctrl Pts',(13.660814864634,2.95701983403981,4.59880705606552));
#14224=CARTESIAN_POINT('Ctrl Pts',(13.665,2.97916814649112,4.6));
#14225=CARTESIAN_POINT('Ctrl Pts',(13.665,3.,4.6));
#14226=CARTESIAN_POINT('Ctrl Pts',(13.335,3.,4.6));
#14227=CARTESIAN_POINT('Ctrl Pts',(13.335,2.97916814649112,4.6));
#14228=CARTESIAN_POINT('Ctrl Pts',(13.339185135366,2.95701983403981,4.59880705606552));
#14229=CARTESIAN_POINT('Ctrl Pts',(13.3546543563418,2.91977655056228,4.59485638705045));
#14230=CARTESIAN_POINT('Ctrl Pts',(13.3646008648105,2.90408240284739,4.59243495840567));
#14231=CARTESIAN_POINT('Ctrl Pts',(13.3762058159686,2.89091287885364,4.59));
#14232=CARTESIAN_POINT('',(13.335,3.,5.));
#14233=CARTESIAN_POINT('',(13.335,3.,4.59));
#14234=CARTESIAN_POINT('Origin',(13.5,3.,5.));
#14235=CARTESIAN_POINT('Origin',(13.5,3.,4.59));
#14236=CARTESIAN_POINT('',(12.9,3.10908712114636,4.59));
#14237=CARTESIAN_POINT('Origin',(13.5,1.9,2.));
#14238=CARTESIAN_POINT('Origin',(13.5,1.9,5.));
#14239=CARTESIAN_POINT('',(13.5,1.5,2.));
#14240=CARTESIAN_POINT('Origin',(13.5,1.9,2.));
#14241=CARTESIAN_POINT('Origin',(13.5,1.9,2.));
#14242=CARTESIAN_POINT('',(13.275,1.9,2.));
#14243=CARTESIAN_POINT('Origin',(13.5,1.9,2.));
#14244=CARTESIAN_POINT('Origin',(13.5,4.1,2.));
#14245=CARTESIAN_POINT('Origin',(13.5,4.1,5.));
#14246=CARTESIAN_POINT('',(13.5,4.5,2.));
#14247=CARTESIAN_POINT('Origin',(13.5,4.1,2.));
#14248=CARTESIAN_POINT('Origin',(13.5,4.1,2.));
#14249=CARTESIAN_POINT('',(13.275,4.1,2.));
#14250=CARTESIAN_POINT('Origin',(13.5,4.1,2.));
#14251=CARTESIAN_POINT('Origin',(13.5,3.,5.));
#14252=CARTESIAN_POINT('',(13.,4.5,5.));
#14253=CARTESIAN_POINT('',(13.,1.5,5.));
#14254=CARTESIAN_POINT('',(13.,4.5,5.));
#14255=CARTESIAN_POINT('',(13.,1.5,5.));
#14256=CARTESIAN_POINT('',(14.,1.5,5.));
#14257=CARTESIAN_POINT('',(13.,1.5,5.));
#14258=CARTESIAN_POINT('',(14.,4.5,5.));
#14259=CARTESIAN_POINT('',(14.,1.5,5.));
#14260=CARTESIAN_POINT('',(14.,4.5,5.));
#14261=CARTESIAN_POINT('',(14.,4.5,5.));
#14262=CARTESIAN_POINT('Origin',(13.5,1.9,0.9));
#14263=CARTESIAN_POINT('',(13.275,1.9,1.));
#14264=CARTESIAN_POINT('Origin',(13.5,1.9,1.));
#14265=CARTESIAN_POINT('',(13.275,1.9,0.9));
#14266=CARTESIAN_POINT('Origin',(13.5,4.1,0.9));
#14267=CARTESIAN_POINT('',(13.275,4.1,1.));
#14268=CARTESIAN_POINT('Origin',(13.5,4.1,1.));
#14269=CARTESIAN_POINT('',(13.275,4.1,0.9));
#14270=CARTESIAN_POINT('Origin',(12.9,3.,4.));
#14271=CARTESIAN_POINT('',(13.,3.,4.6));
#14272=CARTESIAN_POINT('Origin',(13.,3.,4.));
#14273=CARTESIAN_POINT('',(12.9,3.,4.6));
#14274=CARTESIAN_POINT('',(14.,3.,4.6));
#14275=CARTESIAN_POINT('',(12.9,3.,4.6));
#14276=CARTESIAN_POINT('Origin',(14.,3.,4.));
#14277=CARTESIAN_POINT('Origin',(14.,4.5,1.));
#14278=CARTESIAN_POINT('',(14.,4.5,1.));
#14279=CARTESIAN_POINT('',(13.,4.5,1.));
#14280=CARTESIAN_POINT('',(14.,4.5,1.));
#14281=CARTESIAN_POINT('',(13.,4.5,1.));
#14282=CARTESIAN_POINT('',(14.,4.5,1.));
#14283=CARTESIAN_POINT('Origin',(14.,1.5,1.));
#14284=CARTESIAN_POINT('',(14.,1.5,1.));
#14285=CARTESIAN_POINT('',(14.,1.5,1.));
#14286=CARTESIAN_POINT('',(14.,1.5,1.));
#14287=CARTESIAN_POINT('Origin',(13.,1.5,1.));
#14288=CARTESIAN_POINT('',(13.,1.5,1.));
#14289=CARTESIAN_POINT('',(13.,1.5,1.));
#14290=CARTESIAN_POINT('',(13.,1.5,1.));
#14291=CARTESIAN_POINT('Origin',(13.,4.5,1.));
#14292=CARTESIAN_POINT('',(13.,4.5,1.));
#14293=CARTESIAN_POINT('Origin',(13.5,3.,1.));
#14294=CARTESIAN_POINT('',(0.,0.,0.));
#14295=CARTESIAN_POINT('Origin',(-12.4,-1.4142135623731,2.58578643762691));
#14296=CARTESIAN_POINT('',(-12.3,-1.4142135623731,2.75078643762691));
#14297=CARTESIAN_POINT('Origin',(-12.3,-1.4142135623731,2.58578643762691));
#14298=CARTESIAN_POINT('',(-10.7,-1.4142135623731,2.75078643762691));
#14299=CARTESIAN_POINT('',(-12.4,-1.4142135623731,2.75078643762691));
#14300=CARTESIAN_POINT('Origin',(-10.7,-1.4142135623731,2.58578643762691));
#14301=CARTESIAN_POINT('Origin',(-12.4,-1.41421356237309,5.41421356237309));
#14302=CARTESIAN_POINT('',(-12.3,-1.41421356237309,5.57921356237309));
#14303=CARTESIAN_POINT('Origin',(-12.3,-1.41421356237309,5.41421356237309));
#14304=CARTESIAN_POINT('',(-10.7,-1.41421356237309,5.57921356237309));
#14305=CARTESIAN_POINT('',(-12.4,-1.41421356237309,5.57921356237309));
#14306=CARTESIAN_POINT('Origin',(-10.7,-1.41421356237309,5.41421356237309));
#14307=CARTESIAN_POINT('Origin',(-12.4,1.4142135623731,5.41421356237309));
#14308=CARTESIAN_POINT('',(-12.3,1.4142135623731,5.57921356237309));
#14309=CARTESIAN_POINT('Origin',(-12.3,1.4142135623731,5.41421356237309));
#14310=CARTESIAN_POINT('',(-10.7,1.4142135623731,5.57921356237309));
#14311=CARTESIAN_POINT('',(-12.4,1.4142135623731,5.57921356237309));
#14312=CARTESIAN_POINT('Origin',(-10.7,1.4142135623731,5.41421356237309));
#14313=CARTESIAN_POINT('Origin',(-12.4,1.41421356237309,2.5857864376269));
#14314=CARTESIAN_POINT('',(-12.3,1.41421356237309,2.7507864376269));
#14315=CARTESIAN_POINT('Origin',(-12.3,1.41421356237309,2.5857864376269));
#14316=CARTESIAN_POINT('',(-10.7,1.41421356237309,2.7507864376269));
#14317=CARTESIAN_POINT('',(-12.4,1.41421356237309,2.7507864376269));
#14318=CARTESIAN_POINT('Origin',(-10.7,1.41421356237309,2.5857864376269));
#14319=CARTESIAN_POINT('Origin',(-11.5,-3.,0.9));
#14320=CARTESIAN_POINT('',(-11.725,-3.,1.));
#14321=CARTESIAN_POINT('Origin',(-11.5,-3.,1.));
#14322=CARTESIAN_POINT('',(-11.725,-3.,1.8));
#14323=CARTESIAN_POINT('',(-11.725,-3.,0.9));
#14324=CARTESIAN_POINT('Origin',(-11.5,-3.,1.8));
#14325=CARTESIAN_POINT('Origin',(-11.5,3.,0.9));
#14326=CARTESIAN_POINT('',(-11.725,3.,1.));
#14327=CARTESIAN_POINT('Origin',(-11.5,3.,1.));
#14328=CARTESIAN_POINT('',(-11.725,3.,1.8));
#14329=CARTESIAN_POINT('',(-11.725,3.,0.9));
#14330=CARTESIAN_POINT('Origin',(-11.5,3.,1.8));
#14331=CARTESIAN_POINT('Origin',(-12.4,0.,4.));
#14332=CARTESIAN_POINT('',(-12.3,-1.95943487863577E-16,5.6));
#14333=CARTESIAN_POINT('Origin',(-12.3,0.,4.));
#14334=CARTESIAN_POINT('',(-10.7,1.95943487863577E-16,5.6));
#14335=CARTESIAN_POINT('',(-12.4,-1.95943487863577E-16,5.6));
#14336=CARTESIAN_POINT('Origin',(-10.7,0.,4.));
#14337=CARTESIAN_POINT('Origin',(-12.3,3.6,1.8));
#14338=CARTESIAN_POINT('',(-10.7,2.4,1.8));
#14339=CARTESIAN_POINT('',(-12.3,2.4,1.8));
#14340=CARTESIAN_POINT('',(-11.5,2.4,1.8));
#14341=CARTESIAN_POINT('',(-10.7,3.6,1.8));
#14342=CARTESIAN_POINT('',(-10.7,3.6,1.8));
#14343=CARTESIAN_POINT('',(-12.3,3.6,1.8));
#14344=CARTESIAN_POINT('',(-12.3,3.6,1.8));
#14345=CARTESIAN_POINT('',(-12.3,3.6,1.8));
#14346=CARTESIAN_POINT('Origin',(-12.3,3.6,1.8));
#14347=CARTESIAN_POINT('',(-12.3,-2.4,1.8));
#14348=CARTESIAN_POINT('',(-10.7,-2.4,1.8));
#14349=CARTESIAN_POINT('',(-12.3,-2.4,1.8));
#14350=CARTESIAN_POINT('',(-12.3,-3.6,1.8));
#14351=CARTESIAN_POINT('',(-12.3,3.6,1.8));
#14352=CARTESIAN_POINT('',(-10.7,-3.6,1.8));
#14353=CARTESIAN_POINT('',(-12.3,-3.6,1.8));
#14354=CARTESIAN_POINT('',(-10.7,3.6,1.8));
#14355=CARTESIAN_POINT('Origin',(-12.3,3.6,1.));
#14356=CARTESIAN_POINT('',(-12.3,3.6,1.));
#14357=CARTESIAN_POINT('',(-12.3,3.6,1.));
#14358=CARTESIAN_POINT('',(-10.7,3.6,1.));
#14359=CARTESIAN_POINT('',(-10.7,3.6,1.));
#14360=CARTESIAN_POINT('',(-12.3,3.6,1.));
#14361=CARTESIAN_POINT('Origin',(-12.3,-3.6,1.8));
#14362=CARTESIAN_POINT('',(-12.3,-3.6,1.));
#14363=CARTESIAN_POINT('',(-12.3,-3.6,1.8));
#14364=CARTESIAN_POINT('',(-10.7,-3.6,1.));
#14365=CARTESIAN_POINT('',(-12.3,-3.6,1.));
#14366=CARTESIAN_POINT('',(-10.7,-3.6,1.8));
#14367=CARTESIAN_POINT('Origin',(-12.3,-2.4,1.));
#14368=CARTESIAN_POINT('',(-10.7,-2.4,6.5));
#14369=CARTESIAN_POINT('',(-10.7,-2.4,1.));
#14370=CARTESIAN_POINT('',(-12.3,-2.4,6.5));
#14371=CARTESIAN_POINT('',(-12.3,-2.4,6.5));
#14372=CARTESIAN_POINT('',(-12.3,-2.4,1.));
#14373=CARTESIAN_POINT('Origin',(-10.7,-2.4,1.));
#14374=CARTESIAN_POINT('',(-10.7,2.4,6.5));
#14375=CARTESIAN_POINT('',(-10.7,2.4,1.));
#14376=CARTESIAN_POINT('',(-10.7,-2.4,6.5));
#14377=CARTESIAN_POINT('',(-10.7,-3.6,1.));
#14378=CARTESIAN_POINT('Origin',(-10.7,2.4,1.));
#14379=CARTESIAN_POINT('',(-12.3,2.4,6.5));
#14380=CARTESIAN_POINT('',(-12.3,2.4,1.));
#14381=CARTESIAN_POINT('',(-10.7,2.4,6.5));
#14382=CARTESIAN_POINT('Origin',(-12.3,2.4,1.));
#14383=CARTESIAN_POINT('',(-12.3,2.4,6.5));
#14384=CARTESIAN_POINT('',(-12.3,2.4,1.));
#14385=CARTESIAN_POINT('Origin',(-11.5,0.,6.5));
#14386=CARTESIAN_POINT('Origin',(-11.5,0.,1.));
#14387=CARTESIAN_POINT('',(0.,0.,0.));
#14388=CARTESIAN_POINT('Origin',(-12.6,-1.4142135623731,2.58578643762691));
#14389=CARTESIAN_POINT('',(-12.5,-1.4142135623731,2.81078643762691));
#14390=CARTESIAN_POINT('Origin',(-12.5,-1.4142135623731,2.58578643762691));
#14391=CARTESIAN_POINT('',(-12.3,-1.4142135623731,2.81078643762691));
#14392=CARTESIAN_POINT('',(-12.6,-1.4142135623731,2.81078643762691));
#14393=CARTESIAN_POINT('Origin',(-12.3,-1.4142135623731,2.58578643762691));
#14394=CARTESIAN_POINT('Origin',(-12.6,-1.41421356237309,5.41421356237309));
#14395=CARTESIAN_POINT('',(-12.5,-1.41421356237309,5.63921356237309));
#14396=CARTESIAN_POINT('Origin',(-12.5,-1.41421356237309,5.41421356237309));
#14397=CARTESIAN_POINT('',(-12.3,-1.41421356237309,5.63921356237309));
#14398=CARTESIAN_POINT('',(-12.6,-1.41421356237309,5.63921356237309));
#14399=CARTESIAN_POINT('Origin',(-12.3,-1.41421356237309,5.41421356237309));
#14400=CARTESIAN_POINT('Origin',(-12.6,1.4142135623731,5.41421356237309));
#14401=CARTESIAN_POINT('',(-12.5,1.4142135623731,5.63921356237309));
#14402=CARTESIAN_POINT('Origin',(-12.5,1.4142135623731,5.41421356237309));
#14403=CARTESIAN_POINT('',(-12.3,1.4142135623731,5.63921356237309));
#14404=CARTESIAN_POINT('',(-12.6,1.4142135623731,5.63921356237309));
#14405=CARTESIAN_POINT('Origin',(-12.3,1.4142135623731,5.41421356237309));
#14406=CARTESIAN_POINT('Origin',(-12.6,1.41421356237309,2.5857864376269));
#14407=CARTESIAN_POINT('',(-12.5,1.41421356237309,2.8107864376269));
#14408=CARTESIAN_POINT('Origin',(-12.5,1.41421356237309,2.5857864376269));
#14409=CARTESIAN_POINT('',(-12.3,1.41421356237309,2.8107864376269));
#14410=CARTESIAN_POINT('',(-12.6,1.41421356237309,2.8107864376269));
#14411=CARTESIAN_POINT('Origin',(-12.3,1.41421356237309,2.5857864376269));
#14412=CARTESIAN_POINT('Origin',(-12.3,0.,4.));
#14413=CARTESIAN_POINT('',(-12.,-1.94718841064429E-16,5.59));
#14414=CARTESIAN_POINT('Origin',(-12.,0.,4.));
#14415=CARTESIAN_POINT('',(-12.3,-1.94718841064429E-16,5.59));
#14416=CARTESIAN_POINT('',(-12.3,-1.94718841064429E-16,5.59));
#14417=CARTESIAN_POINT('Origin',(-12.3,0.,4.));
#14418=CARTESIAN_POINT('Origin',(-12.,0.,4.));
#14419=CARTESIAN_POINT('',(-12.,-1.23077003314309E-16,5.005));
#14420=CARTESIAN_POINT('Origin',(-12.,0.,4.));
#14421=CARTESIAN_POINT('Origin',(-12.5,0.,4.));
#14422=CARTESIAN_POINT('',(-12.5,-1.23077003314309E-16,5.005));
#14423=CARTESIAN_POINT('',(-12.5,-1.23077003314309E-16,5.005));
#14424=CARTESIAN_POINT('Origin',(-12.5,0.,4.));
#14425=CARTESIAN_POINT('Origin',(-12.5,0.,4.));
#14426=CARTESIAN_POINT('',(-12.3,-2.93915231795365E-16,6.4));
#14427=CARTESIAN_POINT('Origin',(-12.3,0.,4.));
#14428=CARTESIAN_POINT('',(-12.5,-2.93915231795365E-16,6.4));
#14429=CARTESIAN_POINT('',(-12.5,-2.93915231795365E-16,6.4));
#14430=CARTESIAN_POINT('Origin',(-12.5,0.,4.));
#14431=CARTESIAN_POINT('Origin',(-12.3,0.,4.));
#14432=CARTESIAN_POINT('Origin',(-12.5,0.,4.));
#14433=CARTESIAN_POINT('',(0.,0.,0.));
#14434=CARTESIAN_POINT('Origin',(-10.8,-1.4142135623731,2.58578643762691));
#14435=CARTESIAN_POINT('',(-10.7,-1.4142135623731,2.81078643762691));
#14436=CARTESIAN_POINT('Origin',(-10.7,-1.4142135623731,2.58578643762691));
#14437=CARTESIAN_POINT('',(-10.5,-1.4142135623731,2.81078643762691));
#14438=CARTESIAN_POINT('',(-10.8,-1.4142135623731,2.81078643762691));
#14439=CARTESIAN_POINT('Origin',(-10.5,-1.4142135623731,2.58578643762691));
#14440=CARTESIAN_POINT('Origin',(-10.8,-1.41421356237309,5.41421356237309));
#14441=CARTESIAN_POINT('',(-10.7,-1.41421356237309,5.63921356237309));
#14442=CARTESIAN_POINT('Origin',(-10.7,-1.41421356237309,5.41421356237309));
#14443=CARTESIAN_POINT('',(-10.5,-1.41421356237309,5.63921356237309));
#14444=CARTESIAN_POINT('',(-10.8,-1.41421356237309,5.63921356237309));
#14445=CARTESIAN_POINT('Origin',(-10.5,-1.41421356237309,5.41421356237309));
#14446=CARTESIAN_POINT('Origin',(-10.8,1.4142135623731,5.41421356237309));
#14447=CARTESIAN_POINT('',(-10.7,1.4142135623731,5.63921356237309));
#14448=CARTESIAN_POINT('Origin',(-10.7,1.4142135623731,5.41421356237309));
#14449=CARTESIAN_POINT('',(-10.5,1.4142135623731,5.63921356237309));
#14450=CARTESIAN_POINT('',(-10.8,1.4142135623731,5.63921356237309));
#14451=CARTESIAN_POINT('Origin',(-10.5,1.4142135623731,5.41421356237309));
#14452=CARTESIAN_POINT('Origin',(-10.8,1.41421356237309,2.5857864376269));
#14453=CARTESIAN_POINT('',(-10.7,1.41421356237309,2.8107864376269));
#14454=CARTESIAN_POINT('Origin',(-10.7,1.41421356237309,2.5857864376269));
#14455=CARTESIAN_POINT('',(-10.5,1.41421356237309,2.8107864376269));
#14456=CARTESIAN_POINT('',(-10.8,1.41421356237309,2.8107864376269));
#14457=CARTESIAN_POINT('Origin',(-10.5,1.41421356237309,2.5857864376269));
#14458=CARTESIAN_POINT('Origin',(-11.,0.,4.));
#14459=CARTESIAN_POINT('',(-10.7,-1.94718841064429E-16,5.59));
#14460=CARTESIAN_POINT('Origin',(-10.7,0.,4.));
#14461=CARTESIAN_POINT('',(-11.,-1.94718841064429E-16,5.59));
#14462=CARTESIAN_POINT('',(-11.,-1.94718841064429E-16,5.59));
#14463=CARTESIAN_POINT('Origin',(-11.,0.,4.));
#14464=CARTESIAN_POINT('Origin',(-11.,0.,4.));
#14465=CARTESIAN_POINT('',(-11.,-1.23077003314309E-16,5.005));
#14466=CARTESIAN_POINT('Origin',(-11.,0.,4.));
#14467=CARTESIAN_POINT('Origin',(-10.7,0.,4.));
#14468=CARTESIAN_POINT('',(-10.5,-1.23077003314309E-16,5.005));
#14469=CARTESIAN_POINT('Origin',(-10.5,0.,4.));
#14470=CARTESIAN_POINT('',(-10.7,-1.23077003314309E-16,5.005));
#14471=CARTESIAN_POINT('Origin',(-10.7,0.,4.));
#14472=CARTESIAN_POINT('',(-10.5,-2.93915231795365E-16,6.4));
#14473=CARTESIAN_POINT('Origin',(-10.5,0.,4.));
#14474=CARTESIAN_POINT('',(-10.7,-2.93915231795365E-16,6.4));
#14475=CARTESIAN_POINT('',(-10.7,-2.93915231795365E-16,6.4));
#14476=CARTESIAN_POINT('Origin',(-10.7,0.,4.));
#14477=CARTESIAN_POINT('Origin',(-10.5,0.,4.));
#14478=CARTESIAN_POINT('Origin',(-10.7,0.,4.));
#14479=CARTESIAN_POINT('',(0.,0.,0.));
#14480=CARTESIAN_POINT('Origin',(10.6,-1.4142135623731,2.58578643762691));
#14481=CARTESIAN_POINT('',(10.7,-1.4142135623731,2.75078643762691));
#14482=CARTESIAN_POINT('Origin',(10.7,-1.4142135623731,2.58578643762691));
#14483=CARTESIAN_POINT('',(12.3,-1.4142135623731,2.75078643762691));
#14484=CARTESIAN_POINT('',(10.6,-1.4142135623731,2.75078643762691));
#14485=CARTESIAN_POINT('Origin',(12.3,-1.4142135623731,2.58578643762691));
#14486=CARTESIAN_POINT('Origin',(10.6,-1.41421356237309,5.41421356237309));
#14487=CARTESIAN_POINT('',(10.7,-1.41421356237309,5.57921356237309));
#14488=CARTESIAN_POINT('Origin',(10.7,-1.41421356237309,5.41421356237309));
#14489=CARTESIAN_POINT('',(12.3,-1.41421356237309,5.57921356237309));
#14490=CARTESIAN_POINT('',(10.6,-1.41421356237309,5.57921356237309));
#14491=CARTESIAN_POINT('Origin',(12.3,-1.41421356237309,5.41421356237309));
#14492=CARTESIAN_POINT('Origin',(10.6,1.4142135623731,5.41421356237309));
#14493=CARTESIAN_POINT('',(10.7,1.4142135623731,5.57921356237309));
#14494=CARTESIAN_POINT('Origin',(10.7,1.4142135623731,5.41421356237309));
#14495=CARTESIAN_POINT('',(12.3,1.4142135623731,5.57921356237309));
#14496=CARTESIAN_POINT('',(10.6,1.4142135623731,5.57921356237309));
#14497=CARTESIAN_POINT('Origin',(12.3,1.4142135623731,5.41421356237309));
#14498=CARTESIAN_POINT('Origin',(10.6,1.41421356237309,2.5857864376269));
#14499=CARTESIAN_POINT('',(10.7,1.41421356237309,2.7507864376269));
#14500=CARTESIAN_POINT('Origin',(10.7,1.41421356237309,2.5857864376269));
#14501=CARTESIAN_POINT('',(12.3,1.41421356237309,2.7507864376269));
#14502=CARTESIAN_POINT('',(10.6,1.41421356237309,2.7507864376269));
#14503=CARTESIAN_POINT('Origin',(12.3,1.41421356237309,2.5857864376269));
#14504=CARTESIAN_POINT('Origin',(11.5,-3.,0.9));
#14505=CARTESIAN_POINT('',(11.275,-3.,1.));
#14506=CARTESIAN_POINT('Origin',(11.5,-3.,1.));
#14507=CARTESIAN_POINT('',(11.275,-3.,1.8));
#14508=CARTESIAN_POINT('',(11.275,-3.,0.9));
#14509=CARTESIAN_POINT('Origin',(11.5,-3.,1.8));
#14510=CARTESIAN_POINT('Origin',(11.5,3.,0.9));
#14511=CARTESIAN_POINT('',(11.275,3.,1.));
#14512=CARTESIAN_POINT('Origin',(11.5,3.,1.));
#14513=CARTESIAN_POINT('',(11.275,3.,1.8));
#14514=CARTESIAN_POINT('',(11.275,3.,0.9));
#14515=CARTESIAN_POINT('Origin',(11.5,3.,1.8));
#14516=CARTESIAN_POINT('Origin',(10.6,0.,4.));
#14517=CARTESIAN_POINT('',(10.7,-1.95943487863577E-16,5.6));
#14518=CARTESIAN_POINT('Origin',(10.7,0.,4.));
#14519=CARTESIAN_POINT('',(12.3,1.95943487863577E-16,5.6));
#14520=CARTESIAN_POINT('',(10.6,-1.95943487863577E-16,5.6));
#14521=CARTESIAN_POINT('Origin',(12.3,0.,4.));
#14522=CARTESIAN_POINT('Origin',(10.7,3.6,1.8));
#14523=CARTESIAN_POINT('',(12.3,2.4,1.8));
#14524=CARTESIAN_POINT('',(10.7,2.4,1.8));
#14525=CARTESIAN_POINT('',(11.5,2.4,1.8));
#14526=CARTESIAN_POINT('',(12.3,3.6,1.8));
#14527=CARTESIAN_POINT('',(12.3,3.6,1.8));
#14528=CARTESIAN_POINT('',(10.7,3.6,1.8));
#14529=CARTESIAN_POINT('',(10.7,3.6,1.8));
#14530=CARTESIAN_POINT('',(10.7,3.6,1.8));
#14531=CARTESIAN_POINT('Origin',(10.7,3.6,1.8));
#14532=CARTESIAN_POINT('',(10.7,-2.4,1.8));
#14533=CARTESIAN_POINT('',(12.3,-2.4,1.8));
#14534=CARTESIAN_POINT('',(10.7,-2.4,1.8));
#14535=CARTESIAN_POINT('',(10.7,-3.6,1.8));
#14536=CARTESIAN_POINT('',(10.7,3.6,1.8));
#14537=CARTESIAN_POINT('',(12.3,-3.6,1.8));
#14538=CARTESIAN_POINT('',(10.7,-3.6,1.8));
#14539=CARTESIAN_POINT('',(12.3,3.6,1.8));
#14540=CARTESIAN_POINT('Origin',(10.7,3.6,1.));
#14541=CARTESIAN_POINT('',(10.7,3.6,1.));
#14542=CARTESIAN_POINT('',(10.7,3.6,1.));
#14543=CARTESIAN_POINT('',(12.3,3.6,1.));
#14544=CARTESIAN_POINT('',(12.3,3.6,1.));
#14545=CARTESIAN_POINT('',(10.7,3.6,1.));
#14546=CARTESIAN_POINT('Origin',(10.7,-3.6,1.8));
#14547=CARTESIAN_POINT('',(10.7,-3.6,1.));
#14548=CARTESIAN_POINT('',(10.7,-3.6,1.8));
#14549=CARTESIAN_POINT('',(12.3,-3.6,1.));
#14550=CARTESIAN_POINT('',(10.7,-3.6,1.));
#14551=CARTESIAN_POINT('',(12.3,-3.6,1.8));
#14552=CARTESIAN_POINT('Origin',(10.7,-2.4,1.));
#14553=CARTESIAN_POINT('',(12.3,-2.4,6.5));
#14554=CARTESIAN_POINT('',(12.3,-2.4,1.));
#14555=CARTESIAN_POINT('',(10.7,-2.4,6.5));
#14556=CARTESIAN_POINT('',(10.7,-2.4,6.5));
#14557=CARTESIAN_POINT('',(10.7,-2.4,1.));
#14558=CARTESIAN_POINT('Origin',(12.3,-2.4,1.));
#14559=CARTESIAN_POINT('',(12.3,2.4,6.5));
#14560=CARTESIAN_POINT('',(12.3,2.4,1.));
#14561=CARTESIAN_POINT('',(12.3,-2.4,6.5));
#14562=CARTESIAN_POINT('',(12.3,-3.6,1.));
#14563=CARTESIAN_POINT('Origin',(12.3,2.4,1.));
#14564=CARTESIAN_POINT('',(10.7,2.4,6.5));
#14565=CARTESIAN_POINT('',(10.7,2.4,1.));
#14566=CARTESIAN_POINT('',(12.3,2.4,6.5));
#14567=CARTESIAN_POINT('Origin',(10.7,2.4,1.));
#14568=CARTESIAN_POINT('',(10.7,2.4,6.5));
#14569=CARTESIAN_POINT('',(10.7,2.4,1.));
#14570=CARTESIAN_POINT('Origin',(11.5,0.,6.5));
#14571=CARTESIAN_POINT('Origin',(11.5,0.,1.));
#14572=CARTESIAN_POINT('',(0.,0.,0.));
#14573=CARTESIAN_POINT('Origin',(10.4,-1.4142135623731,2.58578643762691));
#14574=CARTESIAN_POINT('',(10.5,-1.4142135623731,2.81078643762691));
#14575=CARTESIAN_POINT('Origin',(10.5,-1.4142135623731,2.58578643762691));
#14576=CARTESIAN_POINT('',(10.7,-1.4142135623731,2.81078643762691));
#14577=CARTESIAN_POINT('',(10.4,-1.4142135623731,2.81078643762691));
#14578=CARTESIAN_POINT('Origin',(10.7,-1.4142135623731,2.58578643762691));
#14579=CARTESIAN_POINT('Origin',(10.4,-1.41421356237309,5.41421356237309));
#14580=CARTESIAN_POINT('',(10.5,-1.41421356237309,5.63921356237309));
#14581=CARTESIAN_POINT('Origin',(10.5,-1.41421356237309,5.41421356237309));
#14582=CARTESIAN_POINT('',(10.7,-1.41421356237309,5.63921356237309));
#14583=CARTESIAN_POINT('',(10.4,-1.41421356237309,5.63921356237309));
#14584=CARTESIAN_POINT('Origin',(10.7,-1.41421356237309,5.41421356237309));
#14585=CARTESIAN_POINT('Origin',(10.4,1.4142135623731,5.41421356237309));
#14586=CARTESIAN_POINT('',(10.5,1.4142135623731,5.63921356237309));
#14587=CARTESIAN_POINT('Origin',(10.5,1.4142135623731,5.41421356237309));
#14588=CARTESIAN_POINT('',(10.7,1.4142135623731,5.63921356237309));
#14589=CARTESIAN_POINT('',(10.4,1.4142135623731,5.63921356237309));
#14590=CARTESIAN_POINT('Origin',(10.7,1.4142135623731,5.41421356237309));
#14591=CARTESIAN_POINT('Origin',(10.4,1.41421356237309,2.5857864376269));
#14592=CARTESIAN_POINT('',(10.5,1.41421356237309,2.8107864376269));
#14593=CARTESIAN_POINT('Origin',(10.5,1.41421356237309,2.5857864376269));
#14594=CARTESIAN_POINT('',(10.7,1.41421356237309,2.8107864376269));
#14595=CARTESIAN_POINT('',(10.4,1.41421356237309,2.8107864376269));
#14596=CARTESIAN_POINT('Origin',(10.7,1.41421356237309,2.5857864376269));
#14597=CARTESIAN_POINT('Origin',(10.7,0.,4.));
#14598=CARTESIAN_POINT('',(11.,-1.94718841064429E-16,5.59));
#14599=CARTESIAN_POINT('Origin',(11.,0.,4.));
#14600=CARTESIAN_POINT('',(10.7,-1.94718841064429E-16,5.59));
#14601=CARTESIAN_POINT('',(10.7,-1.94718841064429E-16,5.59));
#14602=CARTESIAN_POINT('Origin',(10.7,0.,4.));
#14603=CARTESIAN_POINT('Origin',(11.,0.,4.));
#14604=CARTESIAN_POINT('',(11.,-1.23077003314309E-16,5.005));
#14605=CARTESIAN_POINT('Origin',(11.,0.,4.));
#14606=CARTESIAN_POINT('Origin',(10.5,0.,4.));
#14607=CARTESIAN_POINT('',(10.5,-1.23077003314309E-16,5.005));
#14608=CARTESIAN_POINT('',(10.5,-1.23077003314309E-16,5.005));
#14609=CARTESIAN_POINT('Origin',(10.5,0.,4.));
#14610=CARTESIAN_POINT('Origin',(10.5,0.,4.));
#14611=CARTESIAN_POINT('',(10.7,-2.93915231795365E-16,6.4));
#14612=CARTESIAN_POINT('Origin',(10.7,0.,4.));
#14613=CARTESIAN_POINT('',(10.5,-2.93915231795365E-16,6.4));
#14614=CARTESIAN_POINT('',(10.5,-2.93915231795365E-16,6.4));
#14615=CARTESIAN_POINT('Origin',(10.5,0.,4.));
#14616=CARTESIAN_POINT('Origin',(10.7,0.,4.));
#14617=CARTESIAN_POINT('Origin',(10.5,0.,4.));
#14618=CARTESIAN_POINT('',(0.,0.,0.));
#14619=CARTESIAN_POINT('Origin',(12.2,-1.4142135623731,2.58578643762691));
#14620=CARTESIAN_POINT('',(12.3,-1.4142135623731,2.81078643762691));
#14621=CARTESIAN_POINT('Origin',(12.3,-1.4142135623731,2.58578643762691));
#14622=CARTESIAN_POINT('',(12.5,-1.4142135623731,2.81078643762691));
#14623=CARTESIAN_POINT('',(12.2,-1.4142135623731,2.81078643762691));
#14624=CARTESIAN_POINT('Origin',(12.5,-1.4142135623731,2.58578643762691));
#14625=CARTESIAN_POINT('Origin',(12.2,-1.41421356237309,5.41421356237309));
#14626=CARTESIAN_POINT('',(12.3,-1.41421356237309,5.63921356237309));
#14627=CARTESIAN_POINT('Origin',(12.3,-1.41421356237309,5.41421356237309));
#14628=CARTESIAN_POINT('',(12.5,-1.41421356237309,5.63921356237309));
#14629=CARTESIAN_POINT('',(12.2,-1.41421356237309,5.63921356237309));
#14630=CARTESIAN_POINT('Origin',(12.5,-1.41421356237309,5.41421356237309));
#14631=CARTESIAN_POINT('Origin',(12.2,1.4142135623731,5.41421356237309));
#14632=CARTESIAN_POINT('',(12.3,1.4142135623731,5.63921356237309));
#14633=CARTESIAN_POINT('Origin',(12.3,1.4142135623731,5.41421356237309));
#14634=CARTESIAN_POINT('',(12.5,1.4142135623731,5.63921356237309));
#14635=CARTESIAN_POINT('',(12.2,1.4142135623731,5.63921356237309));
#14636=CARTESIAN_POINT('Origin',(12.5,1.4142135623731,5.41421356237309));
#14637=CARTESIAN_POINT('Origin',(12.2,1.41421356237309,2.5857864376269));
#14638=CARTESIAN_POINT('',(12.3,1.41421356237309,2.8107864376269));
#14639=CARTESIAN_POINT('Origin',(12.3,1.41421356237309,2.5857864376269));
#14640=CARTESIAN_POINT('',(12.5,1.41421356237309,2.8107864376269));
#14641=CARTESIAN_POINT('',(12.2,1.41421356237309,2.8107864376269));
#14642=CARTESIAN_POINT('Origin',(12.5,1.41421356237309,2.5857864376269));
#14643=CARTESIAN_POINT('Origin',(12.,0.,4.));
#14644=CARTESIAN_POINT('',(12.3,-1.94718841064429E-16,5.59));
#14645=CARTESIAN_POINT('Origin',(12.3,0.,4.));
#14646=CARTESIAN_POINT('',(12.,-1.94718841064429E-16,5.59));
#14647=CARTESIAN_POINT('',(12.,-1.94718841064429E-16,5.59));
#14648=CARTESIAN_POINT('Origin',(12.,0.,4.));
#14649=CARTESIAN_POINT('Origin',(12.,0.,4.));
#14650=CARTESIAN_POINT('',(12.,-1.23077003314309E-16,5.005));
#14651=CARTESIAN_POINT('Origin',(12.,0.,4.));
#14652=CARTESIAN_POINT('Origin',(12.3,0.,4.));
#14653=CARTESIAN_POINT('',(12.5,-1.23077003314309E-16,5.005));
#14654=CARTESIAN_POINT('Origin',(12.5,0.,4.));
#14655=CARTESIAN_POINT('',(12.3,-1.23077003314309E-16,5.005));
#14656=CARTESIAN_POINT('Origin',(12.3,0.,4.));
#14657=CARTESIAN_POINT('',(12.5,-2.93915231795365E-16,6.4));
#14658=CARTESIAN_POINT('Origin',(12.5,0.,4.));
#14659=CARTESIAN_POINT('',(12.3,-2.93915231795365E-16,6.4));
#14660=CARTESIAN_POINT('',(12.3,-2.93915231795365E-16,6.4));
#14661=CARTESIAN_POINT('Origin',(12.3,0.,4.));
#14662=CARTESIAN_POINT('Origin',(12.5,0.,4.));
#14663=CARTESIAN_POINT('Origin',(12.3,0.,4.));
#14664=CARTESIAN_POINT('',(0.,0.,0.));
#14665=CARTESIAN_POINT('Origin',(0.05,0.,0.));
#14666=CARTESIAN_POINT('',(0.1,7.34788079488412E-17,0.6));
#14667=CARTESIAN_POINT('Origin',(0.1,0.,0.));
#14668=CARTESIAN_POINT('',(0.,-6.12323399573677E-17,0.5));
#14669=CARTESIAN_POINT('',(0.05,-6.73555739531044E-17,0.55));
#14670=CARTESIAN_POINT('Origin',(0.,0.,0.));
#14671=CARTESIAN_POINT('Origin',(0.,0.,0.));
#14672=CARTESIAN_POINT('',(29.9,-7.34788079488412E-17,0.6));
#14673=CARTESIAN_POINT('Origin',(29.9,0.,0.));
#14674=CARTESIAN_POINT('',(0.,-7.34788079488412E-17,0.6));
#14675=CARTESIAN_POINT('Origin',(0.,0.,0.));
#14676=CARTESIAN_POINT('Origin',(29.95,0.,0.));
#14677=CARTESIAN_POINT('',(30.,6.12323399573677E-17,0.5));
#14678=CARTESIAN_POINT('Origin',(30.,0.,0.));
#14679=CARTESIAN_POINT('',(29.95,-6.73555739531044E-17,0.55));
#14680=CARTESIAN_POINT('Origin',(30.,0.,0.));
#14681=CARTESIAN_POINT('',(0.,0.,0.));
#14682=CARTESIAN_POINT('',(0.,0.,0.));
#14683=CARTESIAN_POINT('Origin',(0.,0.,0.));
#14684=CARTESIAN_POINT('',(-1.070235,-0.308121667383195,-1.31065986708547E-16));
#14685=CARTESIAN_POINT('',(-1.31065986708547E-16,-0.308121667383195,1.070235));
#14686=CARTESIAN_POINT('Origin',(0.,-0.308121667383195,0.));
#14687=CARTESIAN_POINT('Origin',(0.,-0.308121667383195,0.));
#14688=CARTESIAN_POINT('',(-1.31065986708547E-16,0.308121667383195,1.070235));
#14689=CARTESIAN_POINT('Origin',(-1.34711147906209E-16,0.,1.1));
#14690=CARTESIAN_POINT('',(-1.070235,0.308121667383195,1.31065986708547E-16));
#14691=CARTESIAN_POINT('Origin',(0.,0.308121667383195,0.));
#14692=CARTESIAN_POINT('Origin',(0.,0.308121667383195,0.));
#14693=CARTESIAN_POINT('Origin',(0.,0.,0.));
#14694=CARTESIAN_POINT('',(-1.070235,0.5,-1.31065986708547E-16));
#14695=CARTESIAN_POINT('',(-1.070235,0.,-1.31065986708547E-16));
#14696=CARTESIAN_POINT('Origin',(0.,0.5,0.));
#14697=CARTESIAN_POINT('Origin',(0.,0.,0.));
#14698=CARTESIAN_POINT('',(-0.6,-0.44,-7.34788079488412E-17));
#14699=CARTESIAN_POINT('Origin',(0.,-0.44,0.));
#14700=CARTESIAN_POINT('',(-0.6,0.44,-7.34788079488412E-17));
#14701=CARTESIAN_POINT('',(-0.6,0.,-7.34788079488412E-17));
#14702=CARTESIAN_POINT('Origin',(0.,0.44,0.));
#14703=CARTESIAN_POINT('Origin',(0.,0.47,0.));
#14704=CARTESIAN_POINT('',(-0.66,0.5,-8.08266887437253E-17));
#14705=CARTESIAN_POINT('',(-0.63,0.47,-7.71527483462832E-17));
#14706=CARTESIAN_POINT('Origin',(0.,0.5,0.));
#14707=CARTESIAN_POINT('Origin',(1.070235,0.5,0.));
#14708=CARTESIAN_POINT('Origin',(0.,0.,0.));
#14709=CARTESIAN_POINT('',(-1.070235,-0.5,-1.31065986708547E-16));
#14710=CARTESIAN_POINT('Origin',(0.,-0.5,0.));
#14711=CARTESIAN_POINT('',(-1.070235,0.,-1.31065986708547E-16));
#14712=CARTESIAN_POINT('Origin',(0.66,-0.5,0.));
#14713=CARTESIAN_POINT('',(-0.66,-0.5,-8.08266887437253E-17));
#14714=CARTESIAN_POINT('Origin',(0.,-0.5,0.));
#14715=CARTESIAN_POINT('Origin',(0.,-0.47,0.));
#14716=CARTESIAN_POINT('',(-0.63,-0.47,-7.71527483462832E-17));
#14717=CARTESIAN_POINT('',(0.,0.,0.));
#14718=CARTESIAN_POINT('Origin',(0.,0.,0.));
#14719=CARTESIAN_POINT('',(-1.129765,0.308121667383195,-1.38356309103871E-16));
#14720=CARTESIAN_POINT('',(-1.38356309103871E-16,0.308121667383195,1.129765));
#14721=CARTESIAN_POINT('Origin',(0.,0.308121667383195,0.));
#14722=CARTESIAN_POINT('Origin',(0.,0.308121667383195,0.));
#14723=CARTESIAN_POINT('',(-1.38356309103871E-16,-0.308121667383195,1.129765));
#14724=CARTESIAN_POINT('Origin',(-1.34711147906209E-16,0.,1.1));
#14725=CARTESIAN_POINT('',(-1.129765,-0.308121667383195,1.38356309103871E-16));
#14726=CARTESIAN_POINT('Origin',(0.,-0.308121667383195,0.));
#14727=CARTESIAN_POINT('Origin',(0.,-0.308121667383195,0.));
#14728=CARTESIAN_POINT('Origin',(0.,0.,0.));
#14729=CARTESIAN_POINT('',(-1.129765,-0.5,-1.38356309103871E-16));
#14730=CARTESIAN_POINT('Origin',(0.,-0.5,0.));
#14731=CARTESIAN_POINT('',(-1.129765,0.,-1.38356309103871E-16));
#14732=CARTESIAN_POINT('Origin',(1.54,0.5,0.));
#14733=CARTESIAN_POINT('',(-1.54,0.5,-1.88595607068692E-16));
#14734=CARTESIAN_POINT('Origin',(0.,0.5,0.));
#14735=CARTESIAN_POINT('',(-1.129765,0.5,-1.38356309103871E-16));
#14736=CARTESIAN_POINT('Origin',(0.,0.5,0.));
#14737=CARTESIAN_POINT('Origin',(0.,0.47,0.));
#14738=CARTESIAN_POINT('',(-1.6,0.44,-1.95943487863577E-16));
#14739=CARTESIAN_POINT('Origin',(0.,0.44,0.));
#14740=CARTESIAN_POINT('',(-1.57,0.47,-1.92269547466134E-16));
#14741=CARTESIAN_POINT('Origin',(0.,0.,0.));
#14742=CARTESIAN_POINT('',(-1.6,-0.44,-1.95943487863577E-16));
#14743=CARTESIAN_POINT('Origin',(0.,-0.44,0.));
#14744=CARTESIAN_POINT('',(-1.6,0.,-1.95943487863577E-16));
#14745=CARTESIAN_POINT('Origin',(0.,-0.47,0.));
#14746=CARTESIAN_POINT('',(-1.54,-0.5,-1.88595607068692E-16));
#14747=CARTESIAN_POINT('Origin',(0.,-0.5,0.));
#14748=CARTESIAN_POINT('',(-1.57,-0.47,-1.92269547466134E-16));
#14749=CARTESIAN_POINT('Origin',(1.129765,-0.5,0.));
#14750=CARTESIAN_POINT('Origin',(0.,0.,0.));
#14751=CARTESIAN_POINT('',(-1.129765,0.,-1.38356309103871E-16));
#14752=CARTESIAN_POINT('',(0.,0.,0.));
#14753=CARTESIAN_POINT('Origin',(1.1,0.,0.));
#14754=CARTESIAN_POINT('',(1.1,-2.23201749654651E-33,0.29765));
#14755=CARTESIAN_POINT('',(1.1,-2.23201749654651E-33,-0.29765));
#14756=CARTESIAN_POINT('Origin',(1.1,0.,0.));
#14757=CARTESIAN_POINT('Origin',(0.685838782044607,0.,-0.860014630714833));
#14758=CARTESIAN_POINT('',(0.918550922801216,-5.31350540756609E-33,-0.674432891191581));
#14759=CARTESIAN_POINT('',(0.453126641287998,8.49470414473068E-34,-1.04559637023808));
#14760=CARTESIAN_POINT('Origin',(0.685838782044607,0.,-0.860014630714833));
#14761=CARTESIAN_POINT('Origin',(-0.244773027351946,0.,-1.07242070340001));
#14762=CARTESIAN_POINT('',(0.0454142657089739,-2.23201749654651E-33,-1.1386540593921));
#14763=CARTESIAN_POINT('',(-0.534960320412865,-2.23201749654651E-33,-1.00618734740791));
#14764=CARTESIAN_POINT('Origin',(-0.244773027351946,0.,-1.07242070340001));
#14765=CARTESIAN_POINT('Origin',(-0.991065754692661,0.,-0.477272113029314));
#14766=CARTESIAN_POINT('',(-0.86192025974432,8.49470414473067E-34,-0.745445496560469));
#14767=CARTESIAN_POINT('',(-1.120211249641,-5.31350540756609E-33,-0.209098729498159));
#14768=CARTESIAN_POINT('Origin',(-0.991065754692661,0.,-0.477272113029314));
#14769=CARTESIAN_POINT('Origin',(-0.991065754692661,0.,0.477272113029314));
#14770=CARTESIAN_POINT('',(-1.120211249641,-2.23201749654651E-33,0.209098729498159));
#14771=CARTESIAN_POINT('',(-0.86192025974432,-2.23201749654651E-33,0.745445496560469));
#14772=CARTESIAN_POINT('Origin',(-0.991065754692661,0.,0.477272113029314));
#14773=CARTESIAN_POINT('Origin',(-0.244773027351946,0.,1.07242070340001));
#14774=CARTESIAN_POINT('',(-0.534960320412866,-2.23201749654651E-33,1.00618734740791));
#14775=CARTESIAN_POINT('',(0.0454142657089737,-2.23201749654651E-33,1.1386540593921));
#14776=CARTESIAN_POINT('Origin',(-0.244773027351946,0.,1.07242070340001));
#14777=CARTESIAN_POINT('Origin',(0.685838782044607,0.,0.860014630714833));
#14778=CARTESIAN_POINT('',(0.453126641287998,-2.23201749654651E-33,1.04559637023808));
#14779=CARTESIAN_POINT('',(0.918550922801216,-2.23201749654651E-33,0.674432891191581));
#14780=CARTESIAN_POINT('Origin',(0.685838782044607,0.,0.860014630714833));
#14781=CARTESIAN_POINT('',(0.,0.,0.));
#14782=CARTESIAN_POINT('Origin',(0.685838782044607,0.,0.860014630714833));
#14783=CARTESIAN_POINT('',(0.413083465285518,-0.05953,0.993751811093549));
#14784=CARTESIAN_POINT('',(0.876916659919095,-0.05953,0.623857181492959));
#14785=CARTESIAN_POINT('Ctrl Pts',(0.413083465285518,-0.05953,0.993751811093549));
#14786=CARTESIAN_POINT('Ctrl Pts',(0.419070565453383,-0.0925528133349865,
0.991263089003441));
#14787=CARTESIAN_POINT('Ctrl Pts',(0.430199341854858,-0.124911173756694,
0.986608710139579));
#14788=CARTESIAN_POINT('Ctrl Pts',(0.457978755888596,-0.177924977804098,
0.973971221090534));
#14789=CARTESIAN_POINT('Ctrl Pts',(0.473077587363685,-0.199697230012983,
0.966820759530997));
#14790=CARTESIAN_POINT('Ctrl Pts',(0.507057380724533,-0.237895043532788,
0.949440676105255));
#14791=CARTESIAN_POINT('Ctrl Pts',(0.525933334162555,-0.254319232363049,
0.939198248544428));
#14792=CARTESIAN_POINT('Ctrl Pts',(0.564362943424238,-0.28018331644634,
0.916597376014514));
#14793=CARTESIAN_POINT('Ctrl Pts',(0.585840553788742,-0.29104845371857,
0.903141581680914));
#14794=CARTESIAN_POINT('Ctrl Pts',(0.629305439856167,-0.30527573347708,
0.873412008702649));
#14795=CARTESIAN_POINT('Ctrl Pts',(0.651278921914856,-0.308638795020976,
0.857118508332695));
#14796=CARTESIAN_POINT('Ctrl Pts',(0.690705563850638,-0.308638795020976,
0.825676810575914));
#14797=CARTESIAN_POINT('Ctrl Pts',(0.711480111898423,-0.30527573347708,
0.807879894508811));
#14798=CARTESIAN_POINT('Ctrl Pts',(0.750136149454208,-0.29104845371857,
0.772120216227122));
#14799=CARTESIAN_POINT('Ctrl Pts',(0.768033796848072,-0.28018331644634,
0.754175290318038));
#14800=CARTESIAN_POINT('Ctrl Pts',(0.798619410861634,-0.254319232363049,
0.721738358858166));
#14801=CARTESIAN_POINT('Ctrl Pts',(0.812805334167529,-0.237895043532788,
0.705614819529209));
#14802=CARTESIAN_POINT('Ctrl Pts',(0.837310877969633,-0.199697230012983,
0.676354402927683));
#14803=CARTESIAN_POINT('Ctrl Pts',(0.847641868610495,-0.177924977804098,
0.663225258065736));
#14804=CARTESIAN_POINT('Ctrl Pts',(0.866144010579847,-0.124911173756694,
0.638954437806245));
#14805=CARTESIAN_POINT('Ctrl Pts',(0.873158080166742,-0.0925528133349865,
0.62914037979579));
#14806=CARTESIAN_POINT('Ctrl Pts',(0.876916659919095,-0.05953,0.623857181492959));
#14807=CARTESIAN_POINT('',(0.437601487681057,-0.05953,1.03511272300331));
#14808=CARTESIAN_POINT('Origin',(0.685838782044607,-0.05953,0.860014630714833));
#14809=CARTESIAN_POINT('',(0.911784794170997,-0.05953,0.656964154625313));
#14810=CARTESIAN_POINT('Ctrl Pts',(0.911784794170998,-0.0595300000000001,
0.656964154625312));
#14811=CARTESIAN_POINT('Ctrl Pts',(0.909827729890942,-0.0762225747374255,
0.659680317203144));
#14812=CARTESIAN_POINT('Ctrl Pts',(0.907004864562642,-0.0928409665394228,
0.663576540841106));
#14813=CARTESIAN_POINT('Ctrl Pts',(0.895234408667242,-0.144299303100741,
0.679480524217551));
#14814=CARTESIAN_POINT('Ctrl Pts',(0.882797231409153,-0.177024326825049,
0.695831250979106));
#14815=CARTESIAN_POINT('Ctrl Pts',(0.854332839576145,-0.227269801620064,
0.73042219438957));
#14816=CARTESIAN_POINT('Ctrl Pts',(0.834863020612702,-0.251265615809407,
0.752807465209441));
#14817=CARTESIAN_POINT('Ctrl Pts',(0.800439809856111,-0.279889827963178,
0.789147407129766));
#14818=CARTESIAN_POINT('Ctrl Pts',(0.781998747691871,-0.290879136862659,
0.80756613568454));
#14819=CARTESIAN_POINT('Ctrl Pts',(0.742239891936898,-0.305251990234487,
0.844254137480382));
#14820=CARTESIAN_POINT('Ctrl Pts',(0.720906778729541,-0.308638795020976,
0.862505527716294));
#14821=CARTESIAN_POINT('Ctrl Pts',(0.680463863683392,-0.308638795020976,
0.894757676234429));
#14822=CARTESIAN_POINT('Ctrl Pts',(0.657923009631182,-0.305251990234488,
0.91149460735272));
#14823=CARTESIAN_POINT('Ctrl Pts',(0.613307674922609,-0.290879136862659,
0.942092777160053));
#14824=CARTESIAN_POINT('Ctrl Pts',(0.591247219971725,-0.279889827963178,
0.955972930713954));
#14825=CARTESIAN_POINT('Ctrl Pts',(0.548158511259202,-0.251265615809407,
0.981446681891443));
#14826=CARTESIAN_POINT('Ctrl Pts',(0.522002043615455,-0.227269801620063,
0.995447160474328));
#14827=CARTESIAN_POINT('Ctrl Pts',(0.481944444320713,-0.177024326825049,
1.01550068154148));
#14828=CARTESIAN_POINT('Ctrl Pts',(0.463236132117164,-0.14429930310074,
1.0239876538093));
#14829=CARTESIAN_POINT('Ctrl Pts',(0.445111721969657,-0.0928409665394226,
1.03192403056628));
#14830=CARTESIAN_POINT('Ctrl Pts',(0.440685038163619,-0.0762225747374254,
1.03380912944435));
#14831=CARTESIAN_POINT('Ctrl Pts',(0.437601487681056,-0.05953,1.03511272300331));
#14832=CARTESIAN_POINT('Origin',(0.685838782044607,-0.05953,0.860014630714833));
#14833=CARTESIAN_POINT('Origin',(0.,-0.208355,0.));
#14834=CARTESIAN_POINT('',(0.0548532617164168,-0.05953,1.12247250791415));
#14835=CARTESIAN_POINT('Origin',(0.,-0.05953,0.));
#14836=CARTESIAN_POINT('',(-0.536443649899848,-0.05953,0.987512846410683));
#14837=CARTESIAN_POINT('Ctrl Pts',(0.0548532617164173,-0.0595300000000001,
1.12247250791414));
#14838=CARTESIAN_POINT('Ctrl Pts',(0.05150947068137,-0.0762225747374254,
1.12263591311425));
#14839=CARTESIAN_POINT('Ctrl Pts',(0.0467032526342597,-0.0928409665394227,
1.12285816383385));
#14840=CARTESIAN_POINT('Ctrl Pts',(0.0269302585198975,-0.144299303100741,
1.12357162229597));
#14841=CARTESIAN_POINT('Ctrl Pts',(0.006392292392153,-0.177024326825049,
1.12404235695137));
#14842=CARTESIAN_POINT('Ctrl Pts',(-0.0383992541984087,-0.227269801620063,
1.12335509974011));
#14843=CARTESIAN_POINT('Ctrl Pts',(-0.0680399972366993,-0.251265615809407,
1.12208997038458));
#14844=CARTESIAN_POINT('Ctrl Pts',(-0.117914228755037,-0.279889827963178,
1.1178344036749));
#14845=CARTESIAN_POINT('Ctrl Pts',(-0.14381238480104,-0.290879136862659,
1.11490049012186));
#14846=CARTESIAN_POINT('Ctrl Pts',(-0.19728546073067,-0.305251990234488,
1.10669035995599));
#14847=CARTESIAN_POINT('Ctrl Pts',(-0.224855950742601,-0.308638795020976,
1.10139101611326));
#14848=CARTESIAN_POINT('Ctrl Pts',(-0.275287440920027,-0.308638795020976,
1.0898803575765));
#14849=CARTESIAN_POINT('Ctrl Pts',(-0.302426893214945,-0.305251990234488,
1.08269251410343));
#14850=CARTESIAN_POINT('Ctrl Pts',(-0.35416671187353,-0.290879136862659,
1.06688848765783));
#14851=CARTESIAN_POINT('Ctrl Pts',(-0.3787731215897,-0.279889827963178,
1.05829506364875));
#14852=CARTESIAN_POINT('Ctrl Pts',(-0.425554672694338,-0.251265615809407,
1.04048957871266));
#14853=CARTESIAN_POINT('Ctrl Pts',(-0.452808978448581,-0.227269801620063,
1.02876878445619));
#14854=CARTESIAN_POINT('Ctrl Pts',(-0.493462957200432,-0.177024326825049,
1.0099536580922));
#14855=CARTESIAN_POINT('Ctrl Pts',(-0.511762781179148,-0.14429930310074,
1.00061845128527));
#14856=CARTESIAN_POINT('Ctrl Pts',(-0.529268075276157,-0.0928409665394226,
0.991396466802468));
#14857=CARTESIAN_POINT('Ctrl Pts',(-0.533501897135713,-0.0762225747374254,
0.989110885965947));
#14858=CARTESIAN_POINT('Ctrl Pts',(-0.536443649899848,-0.0595300000000001,
0.987512846410683));
#14859=CARTESIAN_POINT('',(-0.843383895613249,-0.05953,0.742736168477219));
#14860=CARTESIAN_POINT('Origin',(0.,-0.05953,0.));
#14861=CARTESIAN_POINT('',(-1.10653577764992,-0.05953,0.196295654879792));
#14862=CARTESIAN_POINT('Ctrl Pts',(-0.843383895613249,-0.0595300000000001,
0.742736168477219));
#14863=CARTESIAN_POINT('Ctrl Pts',(-0.84559647055299,-0.0762225747374255,
0.740223768851062));
#14864=CARTESIAN_POINT('Ctrl Pts',(-0.848766861100456,-0.0928409665394227,
0.736604687327351));
#14865=CARTESIAN_POINT('Ctrl Pts',(-0.861652925570091,-0.144299303100741,
0.721590372101268));
#14866=CARTESIAN_POINT('Ctrl Pts',(-0.87482617317514,-0.177024326825049,
0.705826641853758));
#14867=CARTESIAN_POINT('Ctrl Pts',(-0.902215926359523,-0.227269801620063,
0.670378702718353));
#14868=CARTESIAN_POINT('Ctrl Pts',(-0.919707509403859,-0.251265615809407,
0.646415841396062));
#14869=CARTESIAN_POINT('Ctrl Pts',(-0.947476448101718,-0.279889827963178,
0.604769294586516));
#14870=CARTESIAN_POINT('Ctrl Pts',(-0.961329858300736,-0.290879136862659,
0.582692035672022));
#14871=CARTESIAN_POINT('Ctrl Pts',(-0.988250837578047,-0.305251990234488,
0.535766169015486));
#14872=CARTESIAN_POINT('Ctrl Pts',(-1.00129756308006,-0.308638795020976,
0.510906605094603));
#14873=CARTESIAN_POINT('Ctrl Pts',(-1.02374168767024,-0.308638795020976,
0.46430090015576));
#14874=CARTESIAN_POINT('Ctrl Pts',(-1.03504317708586,-0.305251990234488,
0.438600874831839));
#14875=CARTESIAN_POINT('Ctrl Pts',(-1.05494634094458,-0.290879136862659,
0.388295406390235));
#14876=CARTESIAN_POINT('Ctrl Pts',(-1.06356957703048,-0.279889827963178,
0.363699428370917));
#14877=CARTESIAN_POINT('Ctrl Pts',(-1.0788165083757,-0.251265615809407,
0.316022600643821));
#14878=CARTESIAN_POINT('Ctrl Pts',(-1.08664560412098,-0.227269801620063,
0.287406530683752));
#14879=CARTESIAN_POINT('Ctrl Pts',(-1.09728268713976,-0.177024326825049,
0.243890930799337));
#14880=CARTESIAN_POINT('Ctrl Pts',(-1.10139388218929,-0.144299303100741,
0.22376314604679));
#14881=CARTESIAN_POINT('Ctrl Pts',(-1.10509821673782,-0.0928409665394227,
0.204327142733961));
#14882=CARTESIAN_POINT('Ctrl Pts',(-1.10595102243643,-0.0762225747374254,
0.199591971170104));
#14883=CARTESIAN_POINT('Ctrl Pts',(-1.10653577764992,-0.0595300000000001,
0.196295654879792));
#14884=CARTESIAN_POINT('',(-1.123812,-0.05953,1.37627276864339E-16));
#14885=CARTESIAN_POINT('Origin',(0.,-0.05953,0.));
#14886=CARTESIAN_POINT('',(-1.123812,-0.35718,1.37627276864339E-16));
#14887=CARTESIAN_POINT('',(-1.123812,-0.208355,1.37627276864339E-16));
#14888=CARTESIAN_POINT('Origin',(0.,-0.35718,0.));
#14889=CARTESIAN_POINT('',(-1.10653577764992,-0.05953,-0.196295654879793));
#14890=CARTESIAN_POINT('Origin',(0.,-0.05953,0.));
#14891=CARTESIAN_POINT('',(-0.843383895613249,-0.05953,-0.742736168477219));
#14892=CARTESIAN_POINT('Ctrl Pts',(-1.10653577764992,-0.0595300000000001,
-0.196295654879792));
#14893=CARTESIAN_POINT('Ctrl Pts',(-1.10595102243643,-0.0762225747374255,
-0.199591971170104));
#14894=CARTESIAN_POINT('Ctrl Pts',(-1.10509821673782,-0.0928409665394228,
-0.204327142733962));
#14895=CARTESIAN_POINT('Ctrl Pts',(-1.10139388218929,-0.144299303100741,
-0.22376314604679));
#14896=CARTESIAN_POINT('Ctrl Pts',(-1.09728268713976,-0.177024326825049,
-0.243890930799338));
#14897=CARTESIAN_POINT('Ctrl Pts',(-1.08664560412098,-0.227269801620063,
-0.287406530683753));
#14898=CARTESIAN_POINT('Ctrl Pts',(-1.0788165083757,-0.251265615809407,
-0.316022600643821));
#14899=CARTESIAN_POINT('Ctrl Pts',(-1.06356957703048,-0.279889827963178,
-0.363699428370918));
#14900=CARTESIAN_POINT('Ctrl Pts',(-1.05494634094458,-0.290879136862659,
-0.388295406390235));
#14901=CARTESIAN_POINT('Ctrl Pts',(-1.03504317708586,-0.305251990234488,
-0.438600874831839));
#14902=CARTESIAN_POINT('Ctrl Pts',(-1.02374168767024,-0.308638795020976,
-0.46430090015576));
#14903=CARTESIAN_POINT('Ctrl Pts',(-1.00129756308006,-0.308638795020976,
-0.510906605094603));
#14904=CARTESIAN_POINT('Ctrl Pts',(-0.988250837578047,-0.305251990234488,
-0.535766169015486));
#14905=CARTESIAN_POINT('Ctrl Pts',(-0.961329858300736,-0.290879136862659,
-0.582692035672022));
#14906=CARTESIAN_POINT('Ctrl Pts',(-0.947476448101718,-0.279889827963178,
-0.604769294586516));
#14907=CARTESIAN_POINT('Ctrl Pts',(-0.919707509403859,-0.251265615809407,
-0.646415841396062));
#14908=CARTESIAN_POINT('Ctrl Pts',(-0.902215926359523,-0.227269801620064,
-0.670378702718353));
#14909=CARTESIAN_POINT('Ctrl Pts',(-0.87482617317514,-0.177024326825049,
-0.705826641853758));
#14910=CARTESIAN_POINT('Ctrl Pts',(-0.861652925570091,-0.144299303100741,
-0.721590372101268));
#14911=CARTESIAN_POINT('Ctrl Pts',(-0.848766861100456,-0.0928409665394229,
-0.736604687327351));
#14912=CARTESIAN_POINT('Ctrl Pts',(-0.84559647055299,-0.0762225747374255,
-0.740223768851063));
#14913=CARTESIAN_POINT('Ctrl Pts',(-0.843383895613249,-0.0595300000000001,
-0.742736168477219));
#14914=CARTESIAN_POINT('',(-0.536443649899847,-0.05953,-0.987512846410683));
#14915=CARTESIAN_POINT('Origin',(0.,-0.05953,0.));
#14916=CARTESIAN_POINT('',(0.0548532617164172,-0.05953,-1.12247250791415));
#14917=CARTESIAN_POINT('Ctrl Pts',(-0.536443649899848,-0.0595300000000001,
-0.987512846410683));
#14918=CARTESIAN_POINT('Ctrl Pts',(-0.533501897135712,-0.0762225747374254,
-0.989110885965947));
#14919=CARTESIAN_POINT('Ctrl Pts',(-0.529268075276156,-0.0928409665394227,
-0.991396466802469));
#14920=CARTESIAN_POINT('Ctrl Pts',(-0.511762781179147,-0.144299303100741,
-1.00061845128527));
#14921=CARTESIAN_POINT('Ctrl Pts',(-0.493462957200432,-0.177024326825049,
-1.0099536580922));
#14922=CARTESIAN_POINT('Ctrl Pts',(-0.45280897844858,-0.227269801620063,
-1.02876878445619));
#14923=CARTESIAN_POINT('Ctrl Pts',(-0.425554672694337,-0.251265615809407,
-1.04048957871266));
#14924=CARTESIAN_POINT('Ctrl Pts',(-0.3787731215897,-0.279889827963178,
-1.05829506364875));
#14925=CARTESIAN_POINT('Ctrl Pts',(-0.354166711873529,-0.290879136862659,
-1.06688848765783));
#14926=CARTESIAN_POINT('Ctrl Pts',(-0.302426893214944,-0.305251990234488,
-1.08269251410343));
#14927=CARTESIAN_POINT('Ctrl Pts',(-0.275287440920027,-0.308638795020976,
-1.0898803575765));
#14928=CARTESIAN_POINT('Ctrl Pts',(-0.224855950742601,-0.308638795020976,
-1.10139101611326));
#14929=CARTESIAN_POINT('Ctrl Pts',(-0.19728546073067,-0.305251990234488,
-1.10669035995599));
#14930=CARTESIAN_POINT('Ctrl Pts',(-0.143812384801039,-0.290879136862659,
-1.11490049012186));
#14931=CARTESIAN_POINT('Ctrl Pts',(-0.117914228755037,-0.279889827963178,
-1.1178344036749));
#14932=CARTESIAN_POINT('Ctrl Pts',(-0.0680399972366989,-0.251265615809407,
-1.12208997038458));
#14933=CARTESIAN_POINT('Ctrl Pts',(-0.0383992541984084,-0.227269801620063,
-1.12335509974011));
#14934=CARTESIAN_POINT('Ctrl Pts',(0.00639229239215326,-0.177024326825049,
-1.12404235695137));
#14935=CARTESIAN_POINT('Ctrl Pts',(0.0269302585198977,-0.144299303100741,
-1.12357162229597));
#14936=CARTESIAN_POINT('Ctrl Pts',(0.04670325263426,-0.0928409665394228,
-1.12285816383385));
#14937=CARTESIAN_POINT('Ctrl Pts',(0.0515094706813703,-0.0762225747374255,
-1.12263591311425));
#14938=CARTESIAN_POINT('Ctrl Pts',(0.0548532617164176,-0.0595300000000001,
-1.12247250791414));
#14939=CARTESIAN_POINT('',(0.437601487681057,-0.05953,-1.03511272300331));
#14940=CARTESIAN_POINT('Origin',(0.,-0.05953,0.));
#14941=CARTESIAN_POINT('',(0.911784794170997,-0.05953,-0.656964154625313));
#14942=CARTESIAN_POINT('Ctrl Pts',(0.437601487681056,-0.0595300000000001,
-1.03511272300331));
#14943=CARTESIAN_POINT('Ctrl Pts',(0.440685038163619,-0.0762225747374255,
-1.03380912944435));
#14944=CARTESIAN_POINT('Ctrl Pts',(0.445111721969657,-0.0928409665394228,
-1.03192403056628));
#14945=CARTESIAN_POINT('Ctrl Pts',(0.463236132117164,-0.144299303100741,
-1.0239876538093));
#14946=CARTESIAN_POINT('Ctrl Pts',(0.481944444320713,-0.177024326825049,
-1.01550068154148));
#14947=CARTESIAN_POINT('Ctrl Pts',(0.522002043615455,-0.227269801620064,
-0.995447160474328));
#14948=CARTESIAN_POINT('Ctrl Pts',(0.548158511259203,-0.251265615809407,
-0.981446681891443));
#14949=CARTESIAN_POINT('Ctrl Pts',(0.591247219971725,-0.279889827963178,
-0.955972930713954));
#14950=CARTESIAN_POINT('Ctrl Pts',(0.613307674922609,-0.290879136862659,
-0.942092777160053));
#14951=CARTESIAN_POINT('Ctrl Pts',(0.657923009631182,-0.305251990234487,
-0.91149460735272));
#14952=CARTESIAN_POINT('Ctrl Pts',(0.680463863683393,-0.308638795020976,
-0.894757676234429));
#14953=CARTESIAN_POINT('Ctrl Pts',(0.720906778729542,-0.308638795020976,
-0.862505527716294));
#14954=CARTESIAN_POINT('Ctrl Pts',(0.742239891936899,-0.305251990234488,
-0.844254137480381));
#14955=CARTESIAN_POINT('Ctrl Pts',(0.781998747691872,-0.290879136862659,
-0.80756613568454));
#14956=CARTESIAN_POINT('Ctrl Pts',(0.800439809856112,-0.279889827963178,
-0.789147407129765));
#14957=CARTESIAN_POINT('Ctrl Pts',(0.834863020612702,-0.251265615809407,
-0.752807465209441));
#14958=CARTESIAN_POINT('Ctrl Pts',(0.854332839576145,-0.227269801620064,
-0.73042219438957));
#14959=CARTESIAN_POINT('Ctrl Pts',(0.882797231409153,-0.177024326825049,
-0.695831250979106));
#14960=CARTESIAN_POINT('Ctrl Pts',(0.895234408667242,-0.144299303100741,
-0.679480524217551));
#14961=CARTESIAN_POINT('Ctrl Pts',(0.907004864562642,-0.0928409665394228,
-0.663576540841106));
#14962=CARTESIAN_POINT('Ctrl Pts',(0.909827729890942,-0.0762225747374256,
-0.659680317203144));
#14963=CARTESIAN_POINT('Ctrl Pts',(0.911784794170998,-0.0595300000000001,
-0.656964154625312));
#14964=CARTESIAN_POINT('',(1.08212377959455,-0.05953,-0.303251606722892));
#14965=CARTESIAN_POINT('Origin',(0.,-0.05953,0.));
#14966=CARTESIAN_POINT('',(1.08212377959455,-0.05953,0.303251606722892));
#14967=CARTESIAN_POINT('Ctrl Pts',(1.08212377959455,-0.0595300000000001,
-0.303251606722892));
#14968=CARTESIAN_POINT('Ctrl Pts',(1.0830271513892,-0.0762225747374255,
-0.300028012588062));
#14969=CARTESIAN_POINT('Ctrl Pts',(1.08431331394788,-0.0928409665394228,
-0.2953917518996));
#14970=CARTESIAN_POINT('Ctrl Pts',(1.08940878963422,-0.144299303100741,
-0.276273267473431));
#14971=CARTESIAN_POINT('Ctrl Pts',(1.09443784939331,-0.177024326825049,
-0.256354979351213));
#14972=CARTESIAN_POINT('Ctrl Pts',(1.10373487993589,-0.227269801620064,
-0.212533521233765));
#14973=CARTESIAN_POINT('Ctrl Pts',(1.10909715583869,-0.251265615809407,
-0.183354415742157));
#14974=CARTESIAN_POINT('Ctrl Pts',(1.1160463456491,-0.279889827963178,-0.133783682657561));
#14975=CARTESIAN_POINT('Ctrl Pts',(1.11894887330541,-0.290879136862659,
-0.107881990270302));
#14976=CARTESIAN_POINT('Ctrl Pts',(1.12284346704144,-0.305251990234488,
-0.0539226701638766));
#14977=CARTESIAN_POINT('Ctrl Pts',(1.123812,-0.308638795020976,-0.025864214957475));
#14978=CARTESIAN_POINT('Ctrl Pts',(1.123812,-0.308638795020976,0.025864214957475));
#14979=CARTESIAN_POINT('Ctrl Pts',(1.12284346704144,-0.305251990234488,
0.0539226701638766));
#14980=CARTESIAN_POINT('Ctrl Pts',(1.11894887330541,-0.290879136862659,
0.107881990270302));
#14981=CARTESIAN_POINT('Ctrl Pts',(1.1160463456491,-0.279889827963178,0.133783682657561));
#14982=CARTESIAN_POINT('Ctrl Pts',(1.10909715583869,-0.251265615809407,
0.183354415742157));
#14983=CARTESIAN_POINT('Ctrl Pts',(1.10373487993589,-0.227269801620064,
0.212533521233765));
#14984=CARTESIAN_POINT('Ctrl Pts',(1.09443784939331,-0.177024326825049,
0.256354979351213));
#14985=CARTESIAN_POINT('Ctrl Pts',(1.08940878963422,-0.144299303100741,
0.276273267473431));
#14986=CARTESIAN_POINT('Ctrl Pts',(1.08431331394788,-0.0928409665394228,
0.2953917518996));
#14987=CARTESIAN_POINT('Ctrl Pts',(1.0830271513892,-0.0762225747374255,
0.300028012588062));
#14988=CARTESIAN_POINT('Ctrl Pts',(1.08212377959455,-0.0595300000000001,
0.303251606722892));
#14989=CARTESIAN_POINT('Origin',(0.,-0.05953,0.));
#14990=CARTESIAN_POINT('Origin',(0.,-0.05953,0.));
#14991=CARTESIAN_POINT('',(0.0589974094846122,-0.05953,1.07456964270265));
#14992=CARTESIAN_POINT('Origin',(0.,-0.05953,0.));
#14993=CARTESIAN_POINT('Origin',(-0.244773027351946,-0.05953,1.07242070340001));
#14994=CARTESIAN_POINT('Origin',(-0.244773027351946,0.,1.07242070340001));
#14995=CARTESIAN_POINT('',(-0.519393123750572,-0.05953,0.942555777842682));
#14996=CARTESIAN_POINT('Ctrl Pts',(-0.519393123750572,-0.05953,0.942555777842682));
#14997=CARTESIAN_POINT('Ctrl Pts',(-0.513714466572041,-0.0925528133349865,
0.945684988399766));
#14998=CARTESIAN_POINT('Ctrl Pts',(-0.503136848051455,-0.124911173756694,
0.951483858396181));
#14999=CARTESIAN_POINT('Ctrl Pts',(-0.47593627990192,-0.177924977804098,
0.965323333309091));
#15000=CARTESIAN_POINT('Ctrl Pts',(-0.460931856495794,-0.199697230012983,
0.972669835243841));
#15001=CARTESIAN_POINT('Ctrl Pts',(-0.426157505475872,-0.237895043532788,
0.988400002689705));
#15002=CARTESIAN_POINT('Ctrl Pts',(-0.406380688682952,-0.254319232363049,
0.996771768218699));
#15003=CARTESIAN_POINT('Ctrl Pts',(-0.364750145543744,-0.28018331644634,
1.01272583306292));
#15004=CARTESIAN_POINT('Ctrl Pts',(-0.340838910881557,-0.29104845371857,
1.02112815447116));
#15005=CARTESIAN_POINT('Ctrl Pts',(-0.290495481564827,-0.30527573347708,
1.036574285215));
#15006=CARTESIAN_POINT('Ctrl Pts',(-0.264056468041074,-0.308638795020976,
1.04359501395068));
#15007=CARTESIAN_POINT('Ctrl Pts',(-0.214892249704082,-0.308638795020976,
1.05481642595959));
#15008=CARTESIAN_POINT('Ctrl Pts',(-0.188025341585962,-0.30527573347708,
1.05996242598502));
#15009=CARTESIAN_POINT('Ctrl Pts',(-0.135965654106109,-0.29104845371857,
1.06788913840721));
#15010=CARTESIAN_POINT('Ctrl Pts',(-0.110776745452494,-0.28018331644634,
1.07069360430242));
#15011=CARTESIAN_POINT('Ctrl Pts',(-0.0663467128214646,-0.254319232363049,
1.07438230428002));
#15012=CARTESIAN_POINT('Ctrl Pts',(-0.0448960436540983,-0.237895043532788,
1.07542044338697));
#15013=CARTESIAN_POINT('Ctrl Pts',(-0.00674037211528124,-0.199697230012983,
1.07633607767727));
#15014=CARTESIAN_POINT('Ctrl Pts',(0.00996567398334777,-0.177924977804098,
1.07622728347683));
#15015=CARTESIAN_POINT('Ctrl Pts',(0.0404772621979741,-0.124911173756694,
1.07556023164702));
#15016=CARTESIAN_POINT('Ctrl Pts',(0.0525234025782719,-0.0925528133349865,
1.07492508698591));
#15017=CARTESIAN_POINT('Ctrl Pts',(0.0589974094846124,-0.05953,1.07456964270265));
#15018=CARTESIAN_POINT('Origin',(-0.244773027351946,-0.05953,1.07242070340001));
#15019=CARTESIAN_POINT('Origin',(0.,-0.05953,0.));
#15020=CARTESIAN_POINT('',(-0.803348093619616,-0.05953,0.716109245731214));
#15021=CARTESIAN_POINT('Origin',(0.,-0.05953,0.));
#15022=CARTESIAN_POINT('Origin',(-0.991065754692661,-0.05953,0.477272113029314));
#15023=CARTESIAN_POINT('Origin',(-0.991065754692661,0.,0.477272113029314));
#15024=CARTESIAN_POINT('',(-1.06075609691358,-0.05953,0.181596019242328));
#15025=CARTESIAN_POINT('Ctrl Pts',(-1.06075609691358,-0.05953,0.181596019242328));
#15026=CARTESIAN_POINT('Ctrl Pts',(-1.05966202740332,-0.0925528133349865,
0.187986803072856));
#15027=CARTESIAN_POINT('Ctrl Pts',(-1.05760072925372,-0.124911173756694,
0.199872254546857));
#15028=CARTESIAN_POINT('Ctrl Pts',(-1.05146158959546,-0.177924977804098,
0.22976728653846));
#15029=CARTESIAN_POINT('Ctrl Pts',(-1.04785021111757,-0.199697230012983,
0.246078686169301));
#15030=CARTESIAN_POINT('Ctrl Pts',(-1.03846709802406,-0.237895043532788,
0.283073967563097));
#15031=CARTESIAN_POINT('Ctrl Pts',(-1.03268176429485,-0.254319232363049,
0.303755815985685));
#15032=CARTESIAN_POINT('Ctrl Pts',(-1.01919893537026,-0.28018331644634,
0.346251081972725));
#15033=CARTESIAN_POINT('Ctrl Pts',(-1.01085972381132,-0.29104845371857,
0.370184399726282));
#15034=CARTESIAN_POINT('Ctrl Pts',(-0.99154738033959,-0.30527573347708,
0.419174982698463));
#15035=CARTESIAN_POINT('Ctrl Pts',(-0.980551951791748,-0.308638795020976,
0.444223188605045));
#15036=CARTESIAN_POINT('Ctrl Pts',(-0.958671816228589,-0.308638795020976,
0.489657758261848));
#15037=CARTESIAN_POINT('Ctrl Pts',(-0.945943877838127,-0.30527573347708,
0.51387163140139));
#15038=CARTESIAN_POINT('Ctrl Pts',(-0.91968254693063,-0.29104845371857,
0.559515758398093));
#15039=CARTESIAN_POINT('Ctrl Pts',(-0.906170138993533,-0.28018331644634,
0.580957796077825));
#15040=CARTESIAN_POINT('Ctrl Pts',(-0.8813524085237,-0.254319232363049,
0.617994461173994));
#15041=CARTESIAN_POINT('Ctrl Pts',(-0.868789784891799,-0.237895043532788,
0.635412538795143));
#15042=CARTESIAN_POINT('Ctrl Pts',(-0.845715984518854,-0.199697230012983,
0.66581473268113));
#15043=CARTESIAN_POINT('Ctrl Pts',(-0.835214876415962,-0.177924977804098,
0.678808213394124));
#15044=CARTESIAN_POINT('Ctrl Pts',(-0.815669690204649,-0.124911173756694,
0.702247233627224));
#15045=CARTESIAN_POINT('Ctrl Pts',(-0.807662468433796,-0.0925528133349865,
0.711269279199861));
#15046=CARTESIAN_POINT('Ctrl Pts',(-0.803348093619616,-0.05953,0.716109245731214));
#15047=CARTESIAN_POINT('Origin',(-0.991065754692661,-0.05953,0.477272113029314));
#15048=CARTESIAN_POINT('Origin',(0.,-0.05953,0.));
#15049=CARTESIAN_POINT('',(-1.076188,-0.05953,1.31795018948079E-16));
#15050=CARTESIAN_POINT('Origin',(0.,-0.05953,0.));
#15051=CARTESIAN_POINT('',(-1.06075609691358,-0.05953,-0.181596019242328));
#15052=CARTESIAN_POINT('Origin',(0.,-0.05953,0.));
#15053=CARTESIAN_POINT('Origin',(-0.991065754692661,-0.05953,-0.477272113029314));
#15054=CARTESIAN_POINT('Origin',(-0.991065754692661,0.,-0.477272113029314));
#15055=CARTESIAN_POINT('',(-0.803348093619616,-0.05953,-0.716109245731215));
#15056=CARTESIAN_POINT('Ctrl Pts',(-0.803348093619616,-0.05953,-0.716109245731215));
#15057=CARTESIAN_POINT('Ctrl Pts',(-0.807662468433795,-0.0925528133349865,
-0.711269279199862));
#15058=CARTESIAN_POINT('Ctrl Pts',(-0.815669690204649,-0.124911173756694,
-0.702247233627224));
#15059=CARTESIAN_POINT('Ctrl Pts',(-0.835214876415962,-0.177924977804098,
-0.678808213394124));
#15060=CARTESIAN_POINT('Ctrl Pts',(-0.845715984518854,-0.199697230012983,
-0.66581473268113));
#15061=CARTESIAN_POINT('Ctrl Pts',(-0.868789784891799,-0.237895043532788,
-0.635412538795143));
#15062=CARTESIAN_POINT('Ctrl Pts',(-0.8813524085237,-0.254319232363049,
-0.617994461173994));
#15063=CARTESIAN_POINT('Ctrl Pts',(-0.906170138993533,-0.28018331644634,
-0.580957796077826));
#15064=CARTESIAN_POINT('Ctrl Pts',(-0.91968254693063,-0.29104845371857,
-0.559515758398093));
#15065=CARTESIAN_POINT('Ctrl Pts',(-0.945943877838127,-0.30527573347708,
-0.51387163140139));
#15066=CARTESIAN_POINT('Ctrl Pts',(-0.958671816228589,-0.308638795020976,
-0.489657758261848));
#15067=CARTESIAN_POINT('Ctrl Pts',(-0.980551951791748,-0.308638795020976,
-0.444223188605045));
#15068=CARTESIAN_POINT('Ctrl Pts',(-0.99154738033959,-0.30527573347708,
-0.419174982698463));
#15069=CARTESIAN_POINT('Ctrl Pts',(-1.01085972381132,-0.29104845371857,
-0.370184399726282));
#15070=CARTESIAN_POINT('Ctrl Pts',(-1.01919893537026,-0.28018331644634,
-0.346251081972725));
#15071=CARTESIAN_POINT('Ctrl Pts',(-1.03268176429485,-0.254319232363049,
-0.303755815985685));
#15072=CARTESIAN_POINT('Ctrl Pts',(-1.03846709802406,-0.237895043532788,
-0.283073967563097));
#15073=CARTESIAN_POINT('Ctrl Pts',(-1.04785021111757,-0.199697230012983,
-0.246078686169302));
#15074=CARTESIAN_POINT('Ctrl Pts',(-1.05146158959546,-0.177924977804098,
-0.229767286538461));
#15075=CARTESIAN_POINT('Ctrl Pts',(-1.05760072925372,-0.124911173756694,
-0.199872254546858));
#15076=CARTESIAN_POINT('Ctrl Pts',(-1.05966202740332,-0.0925528133349864,
-0.187986803072857));
#15077=CARTESIAN_POINT('Ctrl Pts',(-1.06075609691358,-0.05953,-0.181596019242328));
#15078=CARTESIAN_POINT('Origin',(-0.991065754692661,-0.05953,-0.477272113029314));
#15079=CARTESIAN_POINT('Origin',(0.,-0.05953,0.));
#15080=CARTESIAN_POINT('',(-0.519393123750572,-0.05953,-0.942555777842682));
#15081=CARTESIAN_POINT('Origin',(0.,-0.05953,0.));
#15082=CARTESIAN_POINT('Origin',(-0.244773027351946,-0.05953,-1.07242070340001));
#15083=CARTESIAN_POINT('Origin',(-0.244773027351946,0.,-1.07242070340001));
#15084=CARTESIAN_POINT('',(0.0589974094846125,-0.05953,-1.07456964270265));
#15085=CARTESIAN_POINT('Ctrl Pts',(0.0589974094846127,-0.05953,-1.07456964270265));
#15086=CARTESIAN_POINT('Ctrl Pts',(0.0525234025782722,-0.0925528133349865,
-1.07492508698591));
#15087=CARTESIAN_POINT('Ctrl Pts',(0.0404772621979744,-0.124911173756694,
-1.07556023164702));
#15088=CARTESIAN_POINT('Ctrl Pts',(0.0099656739833481,-0.177924977804098,
-1.07622728347683));
#15089=CARTESIAN_POINT('Ctrl Pts',(-0.00674037211528096,-0.199697230012983,
-1.07633607767727));
#15090=CARTESIAN_POINT('Ctrl Pts',(-0.044896043654098,-0.237895043532788,
-1.07542044338697));
#15091=CARTESIAN_POINT('Ctrl Pts',(-0.0663467128214644,-0.254319232363049,
-1.07438230428002));
#15092=CARTESIAN_POINT('Ctrl Pts',(-0.110776745452493,-0.28018331644634,
-1.07069360430242));
#15093=CARTESIAN_POINT('Ctrl Pts',(-0.135965654106109,-0.29104845371857,
-1.06788913840721));
#15094=CARTESIAN_POINT('Ctrl Pts',(-0.188025341585962,-0.30527573347708,
-1.05996242598502));
#15095=CARTESIAN_POINT('Ctrl Pts',(-0.214892249704082,-0.308638795020976,
-1.05481642595959));
#15096=CARTESIAN_POINT('Ctrl Pts',(-0.264056468041074,-0.308638795020976,
-1.04359501395068));
#15097=CARTESIAN_POINT('Ctrl Pts',(-0.290495481564827,-0.30527573347708,
-1.036574285215));
#15098=CARTESIAN_POINT('Ctrl Pts',(-0.340838910881557,-0.291048453718569,
-1.02112815447116));
#15099=CARTESIAN_POINT('Ctrl Pts',(-0.364750145543744,-0.28018331644634,
-1.01272583306292));
#15100=CARTESIAN_POINT('Ctrl Pts',(-0.406380688682952,-0.254319232363049,
-0.996771768218699));
#15101=CARTESIAN_POINT('Ctrl Pts',(-0.426157505475872,-0.237895043532788,
-0.988400002689705));
#15102=CARTESIAN_POINT('Ctrl Pts',(-0.460931856495794,-0.199697230012983,
-0.972669835243841));
#15103=CARTESIAN_POINT('Ctrl Pts',(-0.475936279901919,-0.177924977804098,
-0.965323333309091));
#15104=CARTESIAN_POINT('Ctrl Pts',(-0.503136848051454,-0.124911173756694,
-0.951483858396181));
#15105=CARTESIAN_POINT('Ctrl Pts',(-0.513714466572041,-0.0925528133349865,
-0.945684988399766));
#15106=CARTESIAN_POINT('Ctrl Pts',(-0.519393123750572,-0.05953,-0.942555777842682));
#15107=CARTESIAN_POINT('Origin',(-0.244773027351946,-0.05953,-1.07242070340001));
#15108=CARTESIAN_POINT('Origin',(0.,-0.05953,0.));
#15109=CARTESIAN_POINT('',(0.413083465285518,-0.05953,-0.993751811093549));
#15110=CARTESIAN_POINT('Origin',(0.,-0.05953,0.));
#15111=CARTESIAN_POINT('Origin',(0.685838782044607,-0.05953,-0.860014630714833));
#15112=CARTESIAN_POINT('Origin',(0.685838782044607,0.,-0.860014630714833));
#15113=CARTESIAN_POINT('',(0.876916659919095,-0.05953,-0.623857181492959));
#15114=CARTESIAN_POINT('Ctrl Pts',(0.876916659919095,-0.05953,-0.623857181492958));
#15115=CARTESIAN_POINT('Ctrl Pts',(0.873158080166742,-0.0925528133349865,
-0.62914037979579));
#15116=CARTESIAN_POINT('Ctrl Pts',(0.866144010579847,-0.124911173756694,
-0.638954437806245));
#15117=CARTESIAN_POINT('Ctrl Pts',(0.847641868610495,-0.177924977804098,
-0.663225258065736));
#15118=CARTESIAN_POINT('Ctrl Pts',(0.837310877969633,-0.199697230012983,
-0.676354402927683));
#15119=CARTESIAN_POINT('Ctrl Pts',(0.81280533416753,-0.237895043532788,
-0.705614819529209));
#15120=CARTESIAN_POINT('Ctrl Pts',(0.798619410861634,-0.254319232363049,
-0.721738358858166));
#15121=CARTESIAN_POINT('Ctrl Pts',(0.768033796848072,-0.28018331644634,
-0.754175290318038));
#15122=CARTESIAN_POINT('Ctrl Pts',(0.750136149454208,-0.29104845371857,
-0.772120216227122));
#15123=CARTESIAN_POINT('Ctrl Pts',(0.711480111898423,-0.30527573347708,
-0.807879894508811));
#15124=CARTESIAN_POINT('Ctrl Pts',(0.690705563850638,-0.308638795020976,
-0.825676810575913));
#15125=CARTESIAN_POINT('Ctrl Pts',(0.651278921914856,-0.308638795020976,
-0.857118508332695));
#15126=CARTESIAN_POINT('Ctrl Pts',(0.629305439856167,-0.30527573347708,
-0.873412008702649));
#15127=CARTESIAN_POINT('Ctrl Pts',(0.585840553788742,-0.29104845371857,
-0.903141581680914));
#15128=CARTESIAN_POINT('Ctrl Pts',(0.564362943424239,-0.28018331644634,
-0.916597376014514));
#15129=CARTESIAN_POINT('Ctrl Pts',(0.525933334162556,-0.254319232363049,
-0.939198248544427));
#15130=CARTESIAN_POINT('Ctrl Pts',(0.507057380724533,-0.237895043532788,
-0.949440676105255));
#15131=CARTESIAN_POINT('Ctrl Pts',(0.473077587363686,-0.199697230012983,
-0.966820759530997));
#15132=CARTESIAN_POINT('Ctrl Pts',(0.457978755888596,-0.177924977804098,
-0.973971221090534));
#15133=CARTESIAN_POINT('Ctrl Pts',(0.430199341854858,-0.124911173756694,
-0.986608710139579));
#15134=CARTESIAN_POINT('Ctrl Pts',(0.419070565453384,-0.0925528133349865,
-0.991263089003441));
#15135=CARTESIAN_POINT('Ctrl Pts',(0.413083465285518,-0.05953,-0.993751811093549));
#15136=CARTESIAN_POINT('Origin',(0.685838782044607,-0.05953,-0.860014630714833));
#15137=CARTESIAN_POINT('Origin',(0.,-0.208355,0.));
#15138=CARTESIAN_POINT('',(-1.076188,-0.35718,1.31795018948079E-16));
#15139=CARTESIAN_POINT('Origin',(0.,-0.35718,0.));
#15140=CARTESIAN_POINT('',(-1.076188,-0.208355,1.31795018948079E-16));
#15141=CARTESIAN_POINT('',(1.03449977959455,-0.05953,0.296632461748266));
#15142=CARTESIAN_POINT('Origin',(0.,-0.05953,0.));
#15143=CARTESIAN_POINT('',(1.03449977959455,-0.05953,-0.296632461748266));
#15144=CARTESIAN_POINT('Ctrl Pts',(1.03449977959455,-0.05953,0.296632461748267));
#15145=CARTESIAN_POINT('Ctrl Pts',(1.03628691421076,-0.0925528133349865,
0.290399865505497));
#15146=CARTESIAN_POINT('Ctrl Pts',(1.03958665287714,-0.124911173756694,
0.278797079997872));
#15147=CARTESIAN_POINT('Ctrl Pts',(1.0470264474309,-0.177924977804098,0.249198913998601));
#15148=CARTESIAN_POINT('Ctrl Pts',(1.05084995891418,-0.199697230012983,
0.232935932341942));
#15149=CARTESIAN_POINT('Ctrl Pts',(1.05844771715377,-0.237895043532788,
0.195533155353269));
#15150=CARTESIAN_POINT('Ctrl Pts',(1.06220882929878,-0.254319232363049,
0.17438929156337));
#15151=CARTESIAN_POINT('Ctrl Pts',(1.06849922508772,-0.28018331644634,0.130252399648131));
#15152=CARTESIAN_POINT('Ctrl Pts',(1.07137013248666,-0.29104845371857,0.105070977154072));
#15153=CARTESIAN_POINT('Ctrl Pts',(1.07522652957392,-0.30527573347708,0.0525526752791107));
#15154=CARTESIAN_POINT('Ctrl Pts',(1.076188,-0.308638795020976,0.025214283908933));
#15155=CARTESIAN_POINT('Ctrl Pts',(1.076188,-0.308638795020976,-0.025214283908933));
#15156=CARTESIAN_POINT('Ctrl Pts',(1.07522652957392,-0.30527573347708,-0.0525526752791107));
#15157=CARTESIAN_POINT('Ctrl Pts',(1.07137013248666,-0.29104845371857,-0.105070977154072));
#15158=CARTESIAN_POINT('Ctrl Pts',(1.06849922508772,-0.28018331644634,-0.130252399648131));
#15159=CARTESIAN_POINT('Ctrl Pts',(1.06220882929878,-0.254319232363049,
-0.17438929156337));
#15160=CARTESIAN_POINT('Ctrl Pts',(1.05844771715377,-0.237895043532788,
-0.195533155353269));
#15161=CARTESIAN_POINT('Ctrl Pts',(1.05084995891418,-0.199697230012983,
-0.232935932341942));
#15162=CARTESIAN_POINT('Ctrl Pts',(1.0470264474309,-0.177924977804098,-0.249198913998601));
#15163=CARTESIAN_POINT('Ctrl Pts',(1.03958665287714,-0.124911173756694,
-0.278797079997872));
#15164=CARTESIAN_POINT('Ctrl Pts',(1.03628691421076,-0.0925528133349865,
-0.290399865505497));
#15165=CARTESIAN_POINT('Ctrl Pts',(1.03449977959455,-0.05953,-0.296632461748267));
#15166=CARTESIAN_POINT('Origin',(0.,-0.05953,0.));
#15167=CARTESIAN_POINT('Origin',(0.,-0.05953,0.));
#15168=CARTESIAN_POINT('Origin',(1.1,-0.05953,0.));
#15169=CARTESIAN_POINT('Origin',(1.1,0.,0.));
#15170=CARTESIAN_POINT('Origin',(1.1,-0.05953,0.));
#15171=CARTESIAN_POINT('Origin',(0.,-0.35718,0.));
#15172=CARTESIAN_POINT('Origin',(0.,-0.05953,0.));
#15173=CARTESIAN_POINT('',(0.,0.,0.));
#15174=CARTESIAN_POINT('Origin',(1.119765,0.495,0.));
#15175=CARTESIAN_POINT('',(-1.119765,0.495,-1.37131662304724E-16));
#15176=CARTESIAN_POINT('Origin',(0.,0.495,0.));
#15177=CARTESIAN_POINT('',(-1.085235,0.495,-1.32902956907268E-16));
#15178=CARTESIAN_POINT('Origin',(0.,0.495,0.));
#15179=CARTESIAN_POINT('Origin',(0.,0.4575,0.));
#15180=CARTESIAN_POINT('',(-1.119765,0.42,-1.37131662304724E-16));
#15181=CARTESIAN_POINT('Origin',(0.,0.42,0.));
#15182=CARTESIAN_POINT('',(-1.119765,0.4575,-1.37131662304724E-16));
#15183=CARTESIAN_POINT('Origin',(1.085235,0.42,0.));
#15184=CARTESIAN_POINT('',(-1.085235,0.42,-1.32902956907268E-16));
#15185=CARTESIAN_POINT('Origin',(0.,0.42,0.));
#15186=CARTESIAN_POINT('Origin',(0.,0.4575,0.));
#15187=CARTESIAN_POINT('',(-1.085235,0.4575,-1.32902956907268E-16));
#15188=CARTESIAN_POINT('Origin',(1.119765,-0.42,0.));
#15189=CARTESIAN_POINT('',(-1.119765,-0.42,-1.37131662304724E-16));
#15190=CARTESIAN_POINT('Origin',(0.,-0.42,0.));
#15191=CARTESIAN_POINT('',(-1.085235,-0.42,-1.32902956907268E-16));
#15192=CARTESIAN_POINT('Origin',(0.,-0.42,0.));
#15193=CARTESIAN_POINT('Origin',(0.,-0.4575,0.));
#15194=CARTESIAN_POINT('',(-1.119765,-0.495,-1.37131662304724E-16));
#15195=CARTESIAN_POINT('Origin',(0.,-0.495,0.));
#15196=CARTESIAN_POINT('',(-1.119765,-0.4575,-1.37131662304724E-16));
#15197=CARTESIAN_POINT('Origin',(1.085235,-0.495,0.));
#15198=CARTESIAN_POINT('',(-1.085235,-0.495,-1.32902956907268E-16));
#15199=CARTESIAN_POINT('Origin',(0.,-0.495,0.));
#15200=CARTESIAN_POINT('Origin',(0.,-0.4575,0.));
#15201=CARTESIAN_POINT('',(-1.085235,-0.4575,-1.32902956907268E-16));
#15202=CARTESIAN_POINT('',(0.,0.,0.));
#15203=CARTESIAN_POINT('',(0.,0.,0.));
#15204=CARTESIAN_POINT('',(0.,0.,0.));
#15205=CARTESIAN_POINT('',(0.,0.,0.));
#15206=CARTESIAN_POINT('',(0.,0.,0.));
#15207=CARTESIAN_POINT('',(0.,0.,0.));
#15208=CARTESIAN_POINT('',(0.,0.,0.));
#15209=CARTESIAN_POINT('Origin',(-6.9,2.5,7.8));
#15210=CARTESIAN_POINT('',(-6.9,2.5,7.965));
#15211=CARTESIAN_POINT('Origin',(-6.9,2.5,7.8));
#15212=CARTESIAN_POINT('',(-5.5,2.5,7.965));
#15213=CARTESIAN_POINT('',(-6.9,2.5,7.965));
#15214=CARTESIAN_POINT('Origin',(-5.5,2.5,7.8));
#15215=CARTESIAN_POINT('Origin',(-6.9,2.5,7.8));
#15216=CARTESIAN_POINT('Origin',(-6.9,-2.5,9.2));
#15217=CARTESIAN_POINT('',(-6.9,-2.5,9.365));
#15218=CARTESIAN_POINT('Origin',(-6.9,-2.5,9.2));
#15219=CARTESIAN_POINT('',(-5.5,-2.5,9.365));
#15220=CARTESIAN_POINT('',(-6.9,-2.5,9.365));
#15221=CARTESIAN_POINT('Origin',(-5.5,-2.5,9.2));
#15222=CARTESIAN_POINT('Origin',(-6.9,-2.5,9.2));
#15223=CARTESIAN_POINT('Origin',(-6.9,-2.5,7.8));
#15224=CARTESIAN_POINT('',(-6.9,-2.5,7.965));
#15225=CARTESIAN_POINT('Origin',(-6.9,-2.5,7.8));
#15226=CARTESIAN_POINT('',(-5.5,-2.5,7.965));
#15227=CARTESIAN_POINT('',(-6.9,-2.5,7.965));
#15228=CARTESIAN_POINT('Origin',(-5.5,-2.5,7.8));
#15229=CARTESIAN_POINT('Origin',(-6.9,-2.5,7.8));
#15230=CARTESIAN_POINT('Origin',(-6.9,2.5,9.2));
#15231=CARTESIAN_POINT('',(-6.9,2.5,9.365));
#15232=CARTESIAN_POINT('Origin',(-6.9,2.5,9.2));
#15233=CARTESIAN_POINT('',(-5.5,2.5,9.365));
#15234=CARTESIAN_POINT('',(-6.9,2.5,9.365));
#15235=CARTESIAN_POINT('Origin',(-5.5,2.5,9.2));
#15236=CARTESIAN_POINT('Origin',(-6.9,2.5,9.2));
#15237=CARTESIAN_POINT('Origin',(-6.4,0.,2.7));
#15238=CARTESIAN_POINT('',(-6.4,-2.02066721859313E-17,2.865));
#15239=CARTESIAN_POINT('Origin',(-6.4,0.,2.7));
#15240=CARTESIAN_POINT('',(-5.5,2.02066721859313E-17,2.865));
#15241=CARTESIAN_POINT('',(-6.4,-2.02066721859313E-17,2.865));
#15242=CARTESIAN_POINT('Origin',(-5.5,0.,2.7));
#15243=CARTESIAN_POINT('Origin',(-6.4,0.,2.7));
#15244=CARTESIAN_POINT('Origin',(-6.4,0.,5.3));
#15245=CARTESIAN_POINT('',(-6.4,-2.02066721859313E-17,5.465));
#15246=CARTESIAN_POINT('Origin',(-6.4,0.,5.3));
#15247=CARTESIAN_POINT('',(-5.5,2.02066721859313E-17,5.465));
#15248=CARTESIAN_POINT('',(-6.4,-2.02066721859313E-17,5.465));
#15249=CARTESIAN_POINT('Origin',(-5.5,0.,5.3));
#15250=CARTESIAN_POINT('Origin',(-6.4,0.,5.3));
#15251=CARTESIAN_POINT('Origin',(-8.6,4.2,3.));
#15252=CARTESIAN_POINT('',(-8.5,4.2,3.165));
#15253=CARTESIAN_POINT('Origin',(-8.5,4.2,3.));
#15254=CARTESIAN_POINT('',(-5.5,4.2,3.165));
#15255=CARTESIAN_POINT('',(-8.6,4.2,3.165));
#15256=CARTESIAN_POINT('Origin',(-5.5,4.2,3.));
#15257=CARTESIAN_POINT('Origin',(-8.6,-4.2,5.8));
#15258=CARTESIAN_POINT('',(-8.5,-4.2,5.965));
#15259=CARTESIAN_POINT('Origin',(-8.5,-4.2,5.8));
#15260=CARTESIAN_POINT('',(-5.5,-4.2,5.965));
#15261=CARTESIAN_POINT('',(-8.6,-4.2,5.965));
#15262=CARTESIAN_POINT('Origin',(-5.5,-4.2,5.8));
#15263=CARTESIAN_POINT('Origin',(-8.6,-4.2,3.));
#15264=CARTESIAN_POINT('',(-8.5,-4.2,3.165));
#15265=CARTESIAN_POINT('Origin',(-8.5,-4.2,3.));
#15266=CARTESIAN_POINT('',(-5.5,-4.2,3.165));
#15267=CARTESIAN_POINT('',(-8.6,-4.2,3.165));
#15268=CARTESIAN_POINT('Origin',(-5.5,-4.2,3.));
#15269=CARTESIAN_POINT('Origin',(-8.6,4.2,5.8));
#15270=CARTESIAN_POINT('',(-8.5,4.2,5.965));
#15271=CARTESIAN_POINT('Origin',(-8.5,4.2,5.8));
#15272=CARTESIAN_POINT('',(-5.5,4.2,5.965));
#15273=CARTESIAN_POINT('',(-8.6,4.2,5.965));
#15274=CARTESIAN_POINT('Origin',(-5.5,4.2,5.8));
#15275=CARTESIAN_POINT('Origin',(-8.6,0.,4.));
#15276=CARTESIAN_POINT('',(-8.5,-1.34711147906209E-16,5.1));
#15277=CARTESIAN_POINT('Origin',(-8.5,0.,4.));
#15278=CARTESIAN_POINT('',(-5.5,1.34711147906209E-16,5.1));
#15279=CARTESIAN_POINT('',(-8.6,-1.34711147906209E-16,5.1));
#15280=CARTESIAN_POINT('Origin',(-5.5,0.,4.));
#15281=CARTESIAN_POINT('Origin',(-8.6,-3.,4.));
#15282=CARTESIAN_POINT('',(-8.5,-3.,5.05));
#15283=CARTESIAN_POINT('Origin',(-8.5,-3.,4.));
#15284=CARTESIAN_POINT('',(-5.5,-3.,5.05));
#15285=CARTESIAN_POINT('',(-8.6,-3.,5.05));
#15286=CARTESIAN_POINT('Origin',(-5.5,-3.,4.));
#15287=CARTESIAN_POINT('Origin',(-8.6,3.,4.));
#15288=CARTESIAN_POINT('',(-8.5,3.,5.05));
#15289=CARTESIAN_POINT('Origin',(-8.5,3.,4.));
#15290=CARTESIAN_POINT('',(-5.5,3.,5.05));
#15291=CARTESIAN_POINT('',(-8.6,3.,5.05));
#15292=CARTESIAN_POINT('Origin',(-5.5,3.,4.));
#15293=CARTESIAN_POINT('Origin',(-5.5,4.7,2.3));
#15294=CARTESIAN_POINT('',(-5.5,4.7,2.3));
#15295=CARTESIAN_POINT('',(-8.5,4.7,2.3));
#15296=CARTESIAN_POINT('',(-5.5,4.7,2.3));
#15297=CARTESIAN_POINT('',(-8.5,4.7,10.));
#15298=CARTESIAN_POINT('',(-8.5,4.7,2.3));
#15299=CARTESIAN_POINT('',(-5.5,4.7,10.));
#15300=CARTESIAN_POINT('',(-5.5,4.7,10.));
#15301=CARTESIAN_POINT('',(-5.5,4.7,2.3));
#15302=CARTESIAN_POINT('Origin',(-5.5,-4.7,2.3));
#15303=CARTESIAN_POINT('',(-5.5,-4.7,2.3));
#15304=CARTESIAN_POINT('',(-5.5,-4.7,2.3));
#15305=CARTESIAN_POINT('',(-5.5,-4.7,10.));
#15306=CARTESIAN_POINT('',(-5.5,-4.7,10.));
#15307=CARTESIAN_POINT('',(-5.5,-4.7,2.3));
#15308=CARTESIAN_POINT('Origin',(-8.5,-4.7,2.3));
#15309=CARTESIAN_POINT('',(-8.5,-4.7,2.3));
#15310=CARTESIAN_POINT('',(-8.5,-4.7,2.3));
#15311=CARTESIAN_POINT('',(-8.5,-4.7,10.));
#15312=CARTESIAN_POINT('',(-8.5,-4.7,10.));
#15313=CARTESIAN_POINT('',(-8.5,-4.7,2.3));
#15314=CARTESIAN_POINT('Origin',(-8.5,4.7,2.3));
#15315=CARTESIAN_POINT('',(-8.5,4.7,2.3));
#15316=CARTESIAN_POINT('',(-8.5,4.7,10.));
#15317=CARTESIAN_POINT('Origin',(-7.,0.,10.));
#15318=CARTESIAN_POINT('Origin',(-7.,0.,2.3));
#15319=CARTESIAN_POINT('',(0.,0.,0.));
#15320=CARTESIAN_POINT('Origin',(-8.9,4.2,3.));
#15321=CARTESIAN_POINT('',(-8.8,4.2,3.225));
#15322=CARTESIAN_POINT('Origin',(-8.8,4.2,3.));
#15323=CARTESIAN_POINT('',(-8.5,4.2,3.225));
#15324=CARTESIAN_POINT('',(-8.9,4.2,3.225));
#15325=CARTESIAN_POINT('Origin',(-8.5,4.2,3.));
#15326=CARTESIAN_POINT('Origin',(-8.9,-4.2,5.8));
#15327=CARTESIAN_POINT('',(-8.8,-4.2,6.025));
#15328=CARTESIAN_POINT('Origin',(-8.8,-4.2,5.8));
#15329=CARTESIAN_POINT('',(-8.5,-4.2,6.025));
#15330=CARTESIAN_POINT('',(-8.9,-4.2,6.025));
#15331=CARTESIAN_POINT('Origin',(-8.5,-4.2,5.8));
#15332=CARTESIAN_POINT('Origin',(-8.9,-4.2,3.));
#15333=CARTESIAN_POINT('',(-8.8,-4.2,3.225));
#15334=CARTESIAN_POINT('Origin',(-8.8,-4.2,3.));
#15335=CARTESIAN_POINT('',(-8.5,-4.2,3.225));
#15336=CARTESIAN_POINT('',(-8.9,-4.2,3.225));
#15337=CARTESIAN_POINT('Origin',(-8.5,-4.2,3.));
#15338=CARTESIAN_POINT('Origin',(-8.9,4.2,5.8));
#15339=CARTESIAN_POINT('',(-8.8,4.2,6.025));
#15340=CARTESIAN_POINT('Origin',(-8.8,4.2,5.8));
#15341=CARTESIAN_POINT('',(-8.5,4.2,6.025));
#15342=CARTESIAN_POINT('',(-8.9,4.2,6.025));
#15343=CARTESIAN_POINT('Origin',(-8.5,4.2,5.8));
#15344=CARTESIAN_POINT('Origin',(-8.9,0.,4.));
#15345=CARTESIAN_POINT('',(-8.8,-2.02066721859313E-16,5.65));
#15346=CARTESIAN_POINT('Origin',(-8.8,0.,4.));
#15347=CARTESIAN_POINT('',(-8.5,2.02066721859313E-16,5.65));
#15348=CARTESIAN_POINT('',(-8.9,-2.02066721859313E-16,5.65));
#15349=CARTESIAN_POINT('Origin',(-8.5,0.,4.));
#15350=CARTESIAN_POINT('Origin',(-8.9,-3.,4.));
#15351=CARTESIAN_POINT('',(-8.8,-3.,4.7));
#15352=CARTESIAN_POINT('Origin',(-8.8,-3.,4.));
#15353=CARTESIAN_POINT('',(-8.5,-3.,4.7));
#15354=CARTESIAN_POINT('',(-8.9,-3.,4.7));
#15355=CARTESIAN_POINT('Origin',(-8.5,-3.,4.));
#15356=CARTESIAN_POINT('Origin',(-8.9,3.,4.));
#15357=CARTESIAN_POINT('',(-8.8,3.,4.7));
#15358=CARTESIAN_POINT('Origin',(-8.8,3.,4.));
#15359=CARTESIAN_POINT('',(-8.5,3.,4.7));
#15360=CARTESIAN_POINT('',(-8.9,3.,4.7));
#15361=CARTESIAN_POINT('Origin',(-8.5,3.,4.));
#15362=CARTESIAN_POINT('Origin',(-8.5,4.7,2.3));
#15363=CARTESIAN_POINT('',(-8.5,4.7,2.3));
#15364=CARTESIAN_POINT('',(-8.8,4.7,2.3));
#15365=CARTESIAN_POINT('',(-8.5,4.7,2.3));
#15366=CARTESIAN_POINT('',(-8.8,4.7,6.5));
#15367=CARTESIAN_POINT('',(-8.8,4.7,2.3));
#15368=CARTESIAN_POINT('',(-8.5,4.7,6.5));
#15369=CARTESIAN_POINT('',(-8.5,4.7,6.5));
#15370=CARTESIAN_POINT('',(-8.5,4.7,2.3));
#15371=CARTESIAN_POINT('Origin',(-8.5,-4.7,2.3));
#15372=CARTESIAN_POINT('',(-8.5,-4.7,2.3));
#15373=CARTESIAN_POINT('',(-8.5,-4.7,2.3));
#15374=CARTESIAN_POINT('',(-8.5,-4.7,6.5));
#15375=CARTESIAN_POINT('',(-8.5,-4.7,6.5));
#15376=CARTESIAN_POINT('',(-8.5,-4.7,2.3));
#15377=CARTESIAN_POINT('Origin',(-8.8,-4.7,2.3));
#15378=CARTESIAN_POINT('',(-8.8,-4.7,2.3));
#15379=CARTESIAN_POINT('',(-8.8,-4.7,2.3));
#15380=CARTESIAN_POINT('',(-8.8,-4.7,6.5));
#15381=CARTESIAN_POINT('',(-8.8,-4.7,6.5));
#15382=CARTESIAN_POINT('',(-8.8,-4.7,2.3));
#15383=CARTESIAN_POINT('Origin',(-8.8,4.7,2.3));
#15384=CARTESIAN_POINT('',(-8.8,4.7,2.3));
#15385=CARTESIAN_POINT('',(-8.8,4.7,6.5));
#15386=CARTESIAN_POINT('Origin',(-8.65,0.,6.5));
#15387=CARTESIAN_POINT('Origin',(-8.65,0.,2.3));
#15388=CARTESIAN_POINT('',(0.,0.,0.));
#15389=CARTESIAN_POINT('Origin',(-5.6,4.2,3.));
#15390=CARTESIAN_POINT('',(-5.5,4.2,3.225));
#15391=CARTESIAN_POINT('Origin',(-5.5,4.2,3.));
#15392=CARTESIAN_POINT('',(-5.2,4.2,3.225));
#15393=CARTESIAN_POINT('',(-5.6,4.2,3.225));
#15394=CARTESIAN_POINT('Origin',(-5.2,4.2,3.));
#15395=CARTESIAN_POINT('Origin',(-5.6,-4.2,5.8));
#15396=CARTESIAN_POINT('',(-5.5,-4.2,6.025));
#15397=CARTESIAN_POINT('Origin',(-5.5,-4.2,5.8));
#15398=CARTESIAN_POINT('',(-5.2,-4.2,6.025));
#15399=CARTESIAN_POINT('',(-5.6,-4.2,6.025));
#15400=CARTESIAN_POINT('Origin',(-5.2,-4.2,5.8));
#15401=CARTESIAN_POINT('Origin',(-5.6,-4.2,3.));
#15402=CARTESIAN_POINT('',(-5.5,-4.2,3.225));
#15403=CARTESIAN_POINT('Origin',(-5.5,-4.2,3.));
#15404=CARTESIAN_POINT('',(-5.2,-4.2,3.225));
#15405=CARTESIAN_POINT('',(-5.6,-4.2,3.225));
#15406=CARTESIAN_POINT('Origin',(-5.2,-4.2,3.));
#15407=CARTESIAN_POINT('Origin',(-5.6,4.2,5.8));
#15408=CARTESIAN_POINT('',(-5.5,4.2,6.025));
#15409=CARTESIAN_POINT('Origin',(-5.5,4.2,5.8));
#15410=CARTESIAN_POINT('',(-5.2,4.2,6.025));
#15411=CARTESIAN_POINT('',(-5.6,4.2,6.025));
#15412=CARTESIAN_POINT('Origin',(-5.2,4.2,5.8));
#15413=CARTESIAN_POINT('Origin',(-5.6,0.,4.));
#15414=CARTESIAN_POINT('',(-5.5,-2.02066721859313E-16,5.65));
#15415=CARTESIAN_POINT('Origin',(-5.5,0.,4.));
#15416=CARTESIAN_POINT('',(-5.2,2.02066721859313E-16,5.65));
#15417=CARTESIAN_POINT('',(-5.6,-2.02066721859313E-16,5.65));
#15418=CARTESIAN_POINT('Origin',(-5.2,0.,4.));
#15419=CARTESIAN_POINT('Origin',(-5.6,-3.,4.));
#15420=CARTESIAN_POINT('',(-5.5,-3.,4.7));
#15421=CARTESIAN_POINT('Origin',(-5.5,-3.,4.));
#15422=CARTESIAN_POINT('',(-5.2,-3.,4.7));
#15423=CARTESIAN_POINT('',(-5.6,-3.,4.7));
#15424=CARTESIAN_POINT('Origin',(-5.2,-3.,4.));
#15425=CARTESIAN_POINT('Origin',(-5.6,3.,4.));
#15426=CARTESIAN_POINT('',(-5.5,3.,4.7));
#15427=CARTESIAN_POINT('Origin',(-5.5,3.,4.));
#15428=CARTESIAN_POINT('',(-5.2,3.,4.7));
#15429=CARTESIAN_POINT('',(-5.6,3.,4.7));
#15430=CARTESIAN_POINT('Origin',(-5.2,3.,4.));
#15431=CARTESIAN_POINT('Origin',(-5.2,4.7,2.3));
#15432=CARTESIAN_POINT('',(-5.2,4.7,2.3));
#15433=CARTESIAN_POINT('',(-5.5,4.7,2.3));
#15434=CARTESIAN_POINT('',(-5.2,4.7,2.3));
#15435=CARTESIAN_POINT('',(-5.5,4.7,6.5));
#15436=CARTESIAN_POINT('',(-5.5,4.7,2.3));
#15437=CARTESIAN_POINT('',(-5.2,4.7,6.5));
#15438=CARTESIAN_POINT('',(-5.2,4.7,6.5));
#15439=CARTESIAN_POINT('',(-5.2,4.7,2.3));
#15440=CARTESIAN_POINT('Origin',(-5.2,-4.7,2.3));
#15441=CARTESIAN_POINT('',(-5.2,-4.7,2.3));
#15442=CARTESIAN_POINT('',(-5.2,-4.7,2.3));
#15443=CARTESIAN_POINT('',(-5.2,-4.7,6.5));
#15444=CARTESIAN_POINT('',(-5.2,-4.7,6.5));
#15445=CARTESIAN_POINT('',(-5.2,-4.7,2.3));
#15446=CARTESIAN_POINT('Origin',(-5.5,-4.7,2.3));
#15447=CARTESIAN_POINT('',(-5.5,-4.7,2.3));
#15448=CARTESIAN_POINT('',(-5.5,-4.7,2.3));
#15449=CARTESIAN_POINT('',(-5.5,-4.7,6.5));
#15450=CARTESIAN_POINT('',(-5.5,-4.7,6.5));
#15451=CARTESIAN_POINT('',(-5.5,-4.7,2.3));
#15452=CARTESIAN_POINT('Origin',(-5.5,4.7,2.3));
#15453=CARTESIAN_POINT('',(-5.5,4.7,2.3));
#15454=CARTESIAN_POINT('',(-5.5,4.7,6.5));
#15455=CARTESIAN_POINT('Origin',(-5.35,0.,6.5));
#15456=CARTESIAN_POINT('Origin',(-5.35,0.,2.3));
#15457=CARTESIAN_POINT('',(0.,0.,0.));
#15458=CARTESIAN_POINT('Origin',(-5.6,0.,2.7));
#15459=CARTESIAN_POINT('',(-5.6,0.0947295350922144,2.90408653846154));
#15460=CARTESIAN_POINT('',(-5.6,-0.0947295350922144,2.90408653846154));
#15461=CARTESIAN_POINT('Origin',(-5.6,0.,4.));
#15462=CARTESIAN_POINT('',(-5.6,-2.75545529808155E-17,2.925));
#15463=CARTESIAN_POINT('Origin',(-5.6,0.,2.7));
#15464=CARTESIAN_POINT('Origin',(-5.6,0.,2.7));
#15465=CARTESIAN_POINT('Origin',(-5.6,0.,2.7));
#15466=CARTESIAN_POINT('',(-5.5,0.0947295350922147,2.90408653846154));
#15467=CARTESIAN_POINT('',(-5.6,0.0947295350922144,2.90408653846154));
#15468=CARTESIAN_POINT('',(-5.5,-0.0947295350922147,2.90408653846154));
#15469=CARTESIAN_POINT('Origin',(-5.5,0.,2.7));
#15470=CARTESIAN_POINT('',(-5.6,-0.0947295350922144,2.90408653846154));
#15471=CARTESIAN_POINT('',(-5.1,2.75545529808155E-17,2.925));
#15472=CARTESIAN_POINT('',(-5.6,-2.75545529808155E-17,2.925));
#15473=CARTESIAN_POINT('Origin',(-5.1,0.,2.7));
#15474=CARTESIAN_POINT('Origin',(-5.6,0.,5.3));
#15475=CARTESIAN_POINT('',(-5.6,-0.0947295350922135,5.09591346153846));
#15476=CARTESIAN_POINT('',(-5.6,-1.34711147906209E-16,5.1));
#15477=CARTESIAN_POINT('Origin',(-5.6,0.,4.));
#15478=CARTESIAN_POINT('',(-5.6,0.0947295350922135,5.09591346153846));
#15479=CARTESIAN_POINT('Origin',(-5.6,0.,5.3));
#15480=CARTESIAN_POINT('Origin',(-5.6,0.,4.));
#15481=CARTESIAN_POINT('Origin',(-5.6,0.,5.3));
#15482=CARTESIAN_POINT('',(-5.5,-0.0947295350922147,5.09591346153846));
#15483=CARTESIAN_POINT('',(-5.6,-0.0947295350922135,5.09591346153846));
#15484=CARTESIAN_POINT('',(-5.5,-2.75545529808154E-17,5.525));
#15485=CARTESIAN_POINT('Origin',(-5.5,0.,5.3));
#15486=CARTESIAN_POINT('',(-5.1,2.75545529808154E-17,5.525));
#15487=CARTESIAN_POINT('',(-5.6,-2.75545529808154E-17,5.525));
#15488=CARTESIAN_POINT('Origin',(-5.1,0.,5.3));
#15489=CARTESIAN_POINT('',(-5.5,0.0947295350922147,5.09591346153846));
#15490=CARTESIAN_POINT('Origin',(-5.5,0.,5.3));
#15491=CARTESIAN_POINT('',(-5.6,0.0947295350922135,5.09591346153846));
#15492=CARTESIAN_POINT('Origin',(-8.5,0.,4.));
#15493=CARTESIAN_POINT('Origin',(-5.5,0.,4.));
#15494=CARTESIAN_POINT('',(-8.5,-1.34711147906209E-16,5.1));
#15495=CARTESIAN_POINT('',(-8.5,-1.34711147906209E-16,5.1));
#15496=CARTESIAN_POINT('Origin',(-8.5,0.,4.));
#15497=CARTESIAN_POINT('Origin',(-5.5,0.,4.));
#15498=CARTESIAN_POINT('Origin',(-5.5,0.,4.));
#15499=CARTESIAN_POINT('',(-5.5,-1.95943487863577E-16,5.6));
#15500=CARTESIAN_POINT('Origin',(-5.5,0.,4.));
#15501=CARTESIAN_POINT('Origin',(-5.5,0.,4.));
#15502=CARTESIAN_POINT('',(-5.1,-1.95943487863577E-16,5.6));
#15503=CARTESIAN_POINT('Origin',(-5.1,0.,4.));
#15504=CARTESIAN_POINT('',(-5.5,-1.95943487863577E-16,5.6));
#15505=CARTESIAN_POINT('Origin',(-5.1,0.,4.));
#15506=CARTESIAN_POINT('',(-5.1,-6.4293956955236E-17,4.525));
#15507=CARTESIAN_POINT('Origin',(-5.1,0.,4.));
#15508=CARTESIAN_POINT('Origin',(-8.5,0.,4.));
#15509=CARTESIAN_POINT('',(-8.5,-6.4293956955236E-17,4.525));
#15510=CARTESIAN_POINT('',(-8.5,-6.4293956955236E-17,4.525));
#15511=CARTESIAN_POINT('Origin',(-8.5,0.,4.));
#15512=CARTESIAN_POINT('Origin',(-8.5,0.,4.));
#15513=CARTESIAN_POINT('',(0.,0.,0.));
#15514=CARTESIAN_POINT('Origin',(-5.2,2.5,7.8));
#15515=CARTESIAN_POINT('',(-5.2,2.5,8.2));
#15516=CARTESIAN_POINT('Origin',(-5.2,2.5,7.8));
#15517=CARTESIAN_POINT('',(-4.8,2.5,8.2));
#15518=CARTESIAN_POINT('',(-5.2,2.5,8.2));
#15519=CARTESIAN_POINT('Origin',(-4.8,2.5,7.8));
#15520=CARTESIAN_POINT('Origin',(-5.2,2.5,7.8));
#15521=CARTESIAN_POINT('',(-5.2,2.5,8.025));
#15522=CARTESIAN_POINT('Origin',(-5.2,2.5,7.8));
#15523=CARTESIAN_POINT('Origin',(-5.2,-2.5,9.2));
#15524=CARTESIAN_POINT('',(-5.2,-2.5,9.6));
#15525=CARTESIAN_POINT('Origin',(-5.2,-2.5,9.2));
#15526=CARTESIAN_POINT('',(-4.8,-2.5,9.6));
#15527=CARTESIAN_POINT('',(-5.2,-2.5,9.6));
#15528=CARTESIAN_POINT('Origin',(-4.8,-2.5,9.2));
#15529=CARTESIAN_POINT('Origin',(-5.2,-2.5,9.2));
#15530=CARTESIAN_POINT('',(-5.2,-2.5,9.425));
#15531=CARTESIAN_POINT('Origin',(-5.2,-2.5,9.2));
#15532=CARTESIAN_POINT('Origin',(-5.2,-2.5,7.8));
#15533=CARTESIAN_POINT('',(-5.2,-2.5,8.2));
#15534=CARTESIAN_POINT('Origin',(-5.2,-2.5,7.8));
#15535=CARTESIAN_POINT('',(-4.8,-2.5,8.2));
#15536=CARTESIAN_POINT('',(-5.2,-2.5,8.2));
#15537=CARTESIAN_POINT('Origin',(-4.8,-2.5,7.8));
#15538=CARTESIAN_POINT('Origin',(-5.2,-2.5,7.8));
#15539=CARTESIAN_POINT('',(-5.2,-2.5,8.025));
#15540=CARTESIAN_POINT('Origin',(-5.2,-2.5,7.8));
#15541=CARTESIAN_POINT('Origin',(-5.2,2.5,9.2));
#15542=CARTESIAN_POINT('',(-5.2,2.5,9.6));
#15543=CARTESIAN_POINT('Origin',(-5.2,2.5,9.2));
#15544=CARTESIAN_POINT('',(-4.8,2.5,9.6));
#15545=CARTESIAN_POINT('',(-5.2,2.5,9.6));
#15546=CARTESIAN_POINT('Origin',(-4.8,2.5,9.2));
#15547=CARTESIAN_POINT('Origin',(-5.2,2.5,9.2));
#15548=CARTESIAN_POINT('',(-5.2,2.5,9.425));
#15549=CARTESIAN_POINT('Origin',(-5.2,2.5,9.2));
#15550=CARTESIAN_POINT('Origin',(-5.6,2.5,7.8));
#15551=CARTESIAN_POINT('',(-5.5,2.5,8.025));
#15552=CARTESIAN_POINT('Origin',(-5.5,2.5,7.8));
#15553=CARTESIAN_POINT('',(-5.6,2.5,8.025));
#15554=CARTESIAN_POINT('Origin',(-5.6,-2.5,9.2));
#15555=CARTESIAN_POINT('',(-5.5,-2.5,9.425));
#15556=CARTESIAN_POINT('Origin',(-5.5,-2.5,9.2));
#15557=CARTESIAN_POINT('',(-5.6,-2.5,9.425));
#15558=CARTESIAN_POINT('Origin',(-5.6,-2.5,7.8));
#15559=CARTESIAN_POINT('',(-5.5,-2.5,8.025));
#15560=CARTESIAN_POINT('Origin',(-5.5,-2.5,7.8));
#15561=CARTESIAN_POINT('',(-5.6,-2.5,8.025));
#15562=CARTESIAN_POINT('Origin',(-5.6,2.5,9.2));
#15563=CARTESIAN_POINT('',(-5.5,2.5,9.425));
#15564=CARTESIAN_POINT('Origin',(-5.5,2.5,9.2));
#15565=CARTESIAN_POINT('',(-5.6,2.5,9.425));
#15566=CARTESIAN_POINT('Origin',(-4.8,4.,7.));
#15567=CARTESIAN_POINT('',(-4.8,4.,7.));
#15568=CARTESIAN_POINT('',(-5.5,4.,7.));
#15569=CARTESIAN_POINT('',(-4.8,4.,7.));
#15570=CARTESIAN_POINT('',(-5.5,4.,10.));
#15571=CARTESIAN_POINT('',(-5.5,4.,7.));
#15572=CARTESIAN_POINT('',(-4.8,4.,10.));
#15573=CARTESIAN_POINT('',(-4.8,4.,10.));
#15574=CARTESIAN_POINT('',(-4.8,4.,7.));
#15575=CARTESIAN_POINT('Origin',(-4.8,-4.,7.));
#15576=CARTESIAN_POINT('',(-4.8,-4.,7.));
#15577=CARTESIAN_POINT('',(-4.8,-4.,7.));
#15578=CARTESIAN_POINT('',(-4.8,-4.,10.));
#15579=CARTESIAN_POINT('',(-4.8,-4.,10.));
#15580=CARTESIAN_POINT('',(-4.8,-4.,7.));
#15581=CARTESIAN_POINT('Origin',(-5.5,-4.,7.));
#15582=CARTESIAN_POINT('',(-5.5,-4.,7.));
#15583=CARTESIAN_POINT('',(-5.5,-4.,7.));
#15584=CARTESIAN_POINT('',(-5.5,-4.,10.));
#15585=CARTESIAN_POINT('',(-5.5,-4.,10.));
#15586=CARTESIAN_POINT('',(-5.5,-4.,7.));
#15587=CARTESIAN_POINT('Origin',(-5.5,4.,7.));
#15588=CARTESIAN_POINT('',(-5.5,4.,7.));
#15589=CARTESIAN_POINT('',(-5.5,4.,10.));
#15590=CARTESIAN_POINT('Origin',(-5.15,0.,10.));
#15591=CARTESIAN_POINT('Origin',(-5.15,0.,7.));
#15592=CARTESIAN_POINT('',(0.,0.,0.));
#15593=CARTESIAN_POINT('',(0.,0.,0.));
#15594=CARTESIAN_POINT('Origin',(5.4,2.5,7.8));
#15595=CARTESIAN_POINT('',(5.5,2.5,7.965));
#15596=CARTESIAN_POINT('Origin',(5.5,2.5,7.8));
#15597=CARTESIAN_POINT('',(6.9,2.5,7.965));
#15598=CARTESIAN_POINT('',(5.4,2.5,7.965));
#15599=CARTESIAN_POINT('Origin',(6.9,2.5,7.8));
#15600=CARTESIAN_POINT('Origin',(6.9,2.5,7.8));
#15601=CARTESIAN_POINT('Origin',(5.4,-2.5,9.2));
#15602=CARTESIAN_POINT('',(5.5,-2.5,9.365));
#15603=CARTESIAN_POINT('Origin',(5.5,-2.5,9.2));
#15604=CARTESIAN_POINT('',(6.9,-2.5,9.365));
#15605=CARTESIAN_POINT('',(5.4,-2.5,9.365));
#15606=CARTESIAN_POINT('Origin',(6.9,-2.5,9.2));
#15607=CARTESIAN_POINT('Origin',(6.9,-2.5,9.2));
#15608=CARTESIAN_POINT('Origin',(5.4,-2.5,7.8));
#15609=CARTESIAN_POINT('',(5.5,-2.5,7.965));
#15610=CARTESIAN_POINT('Origin',(5.5,-2.5,7.8));
#15611=CARTESIAN_POINT('',(6.9,-2.5,7.965));
#15612=CARTESIAN_POINT('',(5.4,-2.5,7.965));
#15613=CARTESIAN_POINT('Origin',(6.9,-2.5,7.8));
#15614=CARTESIAN_POINT('Origin',(6.9,-2.5,7.8));
#15615=CARTESIAN_POINT('Origin',(5.4,2.5,9.2));
#15616=CARTESIAN_POINT('',(5.5,2.5,9.365));
#15617=CARTESIAN_POINT('Origin',(5.5,2.5,9.2));
#15618=CARTESIAN_POINT('',(6.9,2.5,9.365));
#15619=CARTESIAN_POINT('',(5.4,2.5,9.365));
#15620=CARTESIAN_POINT('Origin',(6.9,2.5,9.2));
#15621=CARTESIAN_POINT('Origin',(6.9,2.5,9.2));
#15622=CARTESIAN_POINT('Origin',(5.4,0.,2.7));
#15623=CARTESIAN_POINT('',(5.5,-2.02066721859313E-17,2.865));
#15624=CARTESIAN_POINT('Origin',(5.5,0.,2.7));
#15625=CARTESIAN_POINT('',(6.4,-2.02066721859313E-17,2.865));
#15626=CARTESIAN_POINT('',(5.4,-2.02066721859313E-17,2.865));
#15627=CARTESIAN_POINT('Origin',(6.4,0.,2.7));
#15628=CARTESIAN_POINT('Origin',(6.4,0.,2.7));
#15629=CARTESIAN_POINT('Origin',(5.4,0.,5.3));
#15630=CARTESIAN_POINT('',(5.5,-2.02066721859313E-17,5.465));
#15631=CARTESIAN_POINT('Origin',(5.5,0.,5.3));
#15632=CARTESIAN_POINT('',(6.4,-2.02066721859313E-17,5.465));
#15633=CARTESIAN_POINT('',(5.4,-2.02066721859313E-17,5.465));
#15634=CARTESIAN_POINT('Origin',(6.4,0.,5.3));
#15635=CARTESIAN_POINT('Origin',(6.4,0.,5.3));
#15636=CARTESIAN_POINT('Origin',(5.4,4.2,3.));
#15637=CARTESIAN_POINT('',(5.5,4.2,3.165));
#15638=CARTESIAN_POINT('Origin',(5.5,4.2,3.));
#15639=CARTESIAN_POINT('',(8.5,4.2,3.165));
#15640=CARTESIAN_POINT('',(5.4,4.2,3.165));
#15641=CARTESIAN_POINT('Origin',(8.5,4.2,3.));
#15642=CARTESIAN_POINT('Origin',(5.4,-4.2,5.8));
#15643=CARTESIAN_POINT('',(5.5,-4.2,5.965));
#15644=CARTESIAN_POINT('Origin',(5.5,-4.2,5.8));
#15645=CARTESIAN_POINT('',(8.5,-4.2,5.965));
#15646=CARTESIAN_POINT('',(5.4,-4.2,5.965));
#15647=CARTESIAN_POINT('Origin',(8.5,-4.2,5.8));
#15648=CARTESIAN_POINT('Origin',(5.4,-4.2,3.));
#15649=CARTESIAN_POINT('',(5.5,-4.2,3.165));
#15650=CARTESIAN_POINT('Origin',(5.5,-4.2,3.));
#15651=CARTESIAN_POINT('',(8.5,-4.2,3.165));
#15652=CARTESIAN_POINT('',(5.4,-4.2,3.165));
#15653=CARTESIAN_POINT('Origin',(8.5,-4.2,3.));
#15654=CARTESIAN_POINT('Origin',(5.4,4.2,5.8));
#15655=CARTESIAN_POINT('',(5.5,4.2,5.965));
#15656=CARTESIAN_POINT('Origin',(5.5,4.2,5.8));
#15657=CARTESIAN_POINT('',(8.5,4.2,5.965));
#15658=CARTESIAN_POINT('',(5.4,4.2,5.965));
#15659=CARTESIAN_POINT('Origin',(8.5,4.2,5.8));
#15660=CARTESIAN_POINT('Origin',(5.4,0.,4.));
#15661=CARTESIAN_POINT('',(5.5,-1.34711147906209E-16,5.1));
#15662=CARTESIAN_POINT('Origin',(5.5,0.,4.));
#15663=CARTESIAN_POINT('',(8.5,1.34711147906209E-16,5.1));
#15664=CARTESIAN_POINT('',(5.4,-1.34711147906209E-16,5.1));
#15665=CARTESIAN_POINT('Origin',(8.5,0.,4.));
#15666=CARTESIAN_POINT('Origin',(5.4,-3.,4.));
#15667=CARTESIAN_POINT('',(5.5,-3.,5.05));
#15668=CARTESIAN_POINT('Origin',(5.5,-3.,4.));
#15669=CARTESIAN_POINT('',(8.5,-3.,5.05));
#15670=CARTESIAN_POINT('',(5.4,-3.,5.05));
#15671=CARTESIAN_POINT('Origin',(8.5,-3.,4.));
#15672=CARTESIAN_POINT('Origin',(5.4,3.,4.));
#15673=CARTESIAN_POINT('',(5.5,3.,5.05));
#15674=CARTESIAN_POINT('Origin',(5.5,3.,4.));
#15675=CARTESIAN_POINT('',(8.5,3.,5.05));
#15676=CARTESIAN_POINT('',(5.4,3.,5.05));
#15677=CARTESIAN_POINT('Origin',(8.5,3.,4.));
#15678=CARTESIAN_POINT('Origin',(8.5,4.7,2.3));
#15679=CARTESIAN_POINT('',(8.5,4.7,2.3));
#15680=CARTESIAN_POINT('',(5.5,4.7,2.3));
#15681=CARTESIAN_POINT('',(8.5,4.7,2.3));
#15682=CARTESIAN_POINT('',(5.5,4.7,10.));
#15683=CARTESIAN_POINT('',(5.5,4.7,2.3));
#15684=CARTESIAN_POINT('',(8.5,4.7,10.));
#15685=CARTESIAN_POINT('',(8.5,4.7,10.));
#15686=CARTESIAN_POINT('',(8.5,4.7,2.3));
#15687=CARTESIAN_POINT('Origin',(8.5,-4.7,2.3));
#15688=CARTESIAN_POINT('',(8.5,-4.7,2.3));
#15689=CARTESIAN_POINT('',(8.5,-4.7,2.3));
#15690=CARTESIAN_POINT('',(8.5,-4.7,10.));
#15691=CARTESIAN_POINT('',(8.5,-4.7,10.));
#15692=CARTESIAN_POINT('',(8.5,-4.7,2.3));
#15693=CARTESIAN_POINT('Origin',(5.5,-4.7,2.3));
#15694=CARTESIAN_POINT('',(5.5,-4.7,2.3));
#15695=CARTESIAN_POINT('',(5.5,-4.7,2.3));
#15696=CARTESIAN_POINT('',(5.5,-4.7,10.));
#15697=CARTESIAN_POINT('',(5.5,-4.7,10.));
#15698=CARTESIAN_POINT('',(5.5,-4.7,2.3));
#15699=CARTESIAN_POINT('Origin',(5.5,4.7,2.3));
#15700=CARTESIAN_POINT('',(5.5,4.7,2.3));
#15701=CARTESIAN_POINT('',(5.5,4.7,10.));
#15702=CARTESIAN_POINT('Origin',(7.,0.,10.));
#15703=CARTESIAN_POINT('Origin',(7.,0.,2.3));
#15704=CARTESIAN_POINT('',(0.,0.,0.));
#15705=CARTESIAN_POINT('Origin',(5.1,4.2,3.));
#15706=CARTESIAN_POINT('',(5.2,4.2,3.225));
#15707=CARTESIAN_POINT('Origin',(5.2,4.2,3.));
#15708=CARTESIAN_POINT('',(5.5,4.2,3.225));
#15709=CARTESIAN_POINT('',(5.1,4.2,3.225));
#15710=CARTESIAN_POINT('Origin',(5.5,4.2,3.));
#15711=CARTESIAN_POINT('Origin',(5.1,-4.2,5.8));
#15712=CARTESIAN_POINT('',(5.2,-4.2,6.025));
#15713=CARTESIAN_POINT('Origin',(5.2,-4.2,5.8));
#15714=CARTESIAN_POINT('',(5.5,-4.2,6.025));
#15715=CARTESIAN_POINT('',(5.1,-4.2,6.025));
#15716=CARTESIAN_POINT('Origin',(5.5,-4.2,5.8));
#15717=CARTESIAN_POINT('Origin',(5.1,-4.2,3.));
#15718=CARTESIAN_POINT('',(5.2,-4.2,3.225));
#15719=CARTESIAN_POINT('Origin',(5.2,-4.2,3.));
#15720=CARTESIAN_POINT('',(5.5,-4.2,3.225));
#15721=CARTESIAN_POINT('',(5.1,-4.2,3.225));
#15722=CARTESIAN_POINT('Origin',(5.5,-4.2,3.));
#15723=CARTESIAN_POINT('Origin',(5.1,4.2,5.8));
#15724=CARTESIAN_POINT('',(5.2,4.2,6.025));
#15725=CARTESIAN_POINT('Origin',(5.2,4.2,5.8));
#15726=CARTESIAN_POINT('',(5.5,4.2,6.025));
#15727=CARTESIAN_POINT('',(5.1,4.2,6.025));
#15728=CARTESIAN_POINT('Origin',(5.5,4.2,5.8));
#15729=CARTESIAN_POINT('Origin',(5.1,0.,4.));
#15730=CARTESIAN_POINT('',(5.2,-2.02066721859313E-16,5.65));
#15731=CARTESIAN_POINT('Origin',(5.2,0.,4.));
#15732=CARTESIAN_POINT('',(5.5,2.02066721859313E-16,5.65));
#15733=CARTESIAN_POINT('',(5.1,-2.02066721859313E-16,5.65));
#15734=CARTESIAN_POINT('Origin',(5.5,0.,4.));
#15735=CARTESIAN_POINT('Origin',(5.1,-3.,4.));
#15736=CARTESIAN_POINT('',(5.2,-3.,4.7));
#15737=CARTESIAN_POINT('Origin',(5.2,-3.,4.));
#15738=CARTESIAN_POINT('',(5.5,-3.,4.7));
#15739=CARTESIAN_POINT('',(5.1,-3.,4.7));
#15740=CARTESIAN_POINT('Origin',(5.5,-3.,4.));
#15741=CARTESIAN_POINT('Origin',(5.1,3.,4.));
#15742=CARTESIAN_POINT('',(5.2,3.,4.7));
#15743=CARTESIAN_POINT('Origin',(5.2,3.,4.));
#15744=CARTESIAN_POINT('',(5.5,3.,4.7));
#15745=CARTESIAN_POINT('',(5.1,3.,4.7));
#15746=CARTESIAN_POINT('Origin',(5.5,3.,4.));
#15747=CARTESIAN_POINT('Origin',(5.5,4.7,2.3));
#15748=CARTESIAN_POINT('',(5.5,4.7,2.3));
#15749=CARTESIAN_POINT('',(5.2,4.7,2.3));
#15750=CARTESIAN_POINT('',(5.5,4.7,2.3));
#15751=CARTESIAN_POINT('',(5.2,4.7,6.5));
#15752=CARTESIAN_POINT('',(5.2,4.7,2.3));
#15753=CARTESIAN_POINT('',(5.5,4.7,6.5));
#15754=CARTESIAN_POINT('',(5.5,4.7,6.5));
#15755=CARTESIAN_POINT('',(5.5,4.7,2.3));
#15756=CARTESIAN_POINT('Origin',(5.5,-4.7,2.3));
#15757=CARTESIAN_POINT('',(5.5,-4.7,2.3));
#15758=CARTESIAN_POINT('',(5.5,-4.7,2.3));
#15759=CARTESIAN_POINT('',(5.5,-4.7,6.5));
#15760=CARTESIAN_POINT('',(5.5,-4.7,6.5));
#15761=CARTESIAN_POINT('',(5.5,-4.7,2.3));
#15762=CARTESIAN_POINT('Origin',(5.2,-4.7,2.3));
#15763=CARTESIAN_POINT('',(5.2,-4.7,2.3));
#15764=CARTESIAN_POINT('',(5.2,-4.7,2.3));
#15765=CARTESIAN_POINT('',(5.2,-4.7,6.5));
#15766=CARTESIAN_POINT('',(5.2,-4.7,6.5));
#15767=CARTESIAN_POINT('',(5.2,-4.7,2.3));
#15768=CARTESIAN_POINT('Origin',(5.2,4.7,2.3));
#15769=CARTESIAN_POINT('',(5.2,4.7,2.3));
#15770=CARTESIAN_POINT('',(5.2,4.7,6.5));
#15771=CARTESIAN_POINT('Origin',(5.35,0.,6.5));
#15772=CARTESIAN_POINT('Origin',(5.35,0.,2.3));
#15773=CARTESIAN_POINT('',(0.,0.,0.));
#15774=CARTESIAN_POINT('Origin',(8.4,4.2,3.));
#15775=CARTESIAN_POINT('',(8.5,4.2,3.225));
#15776=CARTESIAN_POINT('Origin',(8.5,4.2,3.));
#15777=CARTESIAN_POINT('',(8.8,4.2,3.225));
#15778=CARTESIAN_POINT('',(8.4,4.2,3.225));
#15779=CARTESIAN_POINT('Origin',(8.8,4.2,3.));
#15780=CARTESIAN_POINT('Origin',(8.4,-4.2,5.8));
#15781=CARTESIAN_POINT('',(8.5,-4.2,6.025));
#15782=CARTESIAN_POINT('Origin',(8.5,-4.2,5.8));
#15783=CARTESIAN_POINT('',(8.8,-4.2,6.025));
#15784=CARTESIAN_POINT('',(8.4,-4.2,6.025));
#15785=CARTESIAN_POINT('Origin',(8.8,-4.2,5.8));
#15786=CARTESIAN_POINT('Origin',(8.4,-4.2,3.));
#15787=CARTESIAN_POINT('',(8.5,-4.2,3.225));
#15788=CARTESIAN_POINT('Origin',(8.5,-4.2,3.));
#15789=CARTESIAN_POINT('',(8.8,-4.2,3.225));
#15790=CARTESIAN_POINT('',(8.4,-4.2,3.225));
#15791=CARTESIAN_POINT('Origin',(8.8,-4.2,3.));
#15792=CARTESIAN_POINT('Origin',(8.4,4.2,5.8));
#15793=CARTESIAN_POINT('',(8.5,4.2,6.025));
#15794=CARTESIAN_POINT('Origin',(8.5,4.2,5.8));
#15795=CARTESIAN_POINT('',(8.8,4.2,6.025));
#15796=CARTESIAN_POINT('',(8.4,4.2,6.025));
#15797=CARTESIAN_POINT('Origin',(8.8,4.2,5.8));
#15798=CARTESIAN_POINT('Origin',(8.4,0.,4.));
#15799=CARTESIAN_POINT('',(8.5,-2.02066721859313E-16,5.65));
#15800=CARTESIAN_POINT('Origin',(8.5,0.,4.));
#15801=CARTESIAN_POINT('',(8.8,2.02066721859313E-16,5.65));
#15802=CARTESIAN_POINT('',(8.4,-2.02066721859313E-16,5.65));
#15803=CARTESIAN_POINT('Origin',(8.8,0.,4.));
#15804=CARTESIAN_POINT('Origin',(8.4,-3.,4.));
#15805=CARTESIAN_POINT('',(8.5,-3.,4.7));
#15806=CARTESIAN_POINT('Origin',(8.5,-3.,4.));
#15807=CARTESIAN_POINT('',(8.8,-3.,4.7));
#15808=CARTESIAN_POINT('',(8.4,-3.,4.7));
#15809=CARTESIAN_POINT('Origin',(8.8,-3.,4.));
#15810=CARTESIAN_POINT('Origin',(8.4,3.,4.));
#15811=CARTESIAN_POINT('',(8.5,3.,4.7));
#15812=CARTESIAN_POINT('Origin',(8.5,3.,4.));
#15813=CARTESIAN_POINT('',(8.8,3.,4.7));
#15814=CARTESIAN_POINT('',(8.4,3.,4.7));
#15815=CARTESIAN_POINT('Origin',(8.8,3.,4.));
#15816=CARTESIAN_POINT('Origin',(8.8,4.7,2.3));
#15817=CARTESIAN_POINT('',(8.8,4.7,2.3));
#15818=CARTESIAN_POINT('',(8.5,4.7,2.3));
#15819=CARTESIAN_POINT('',(8.8,4.7,2.3));
#15820=CARTESIAN_POINT('',(8.5,4.7,6.5));
#15821=CARTESIAN_POINT('',(8.5,4.7,2.3));
#15822=CARTESIAN_POINT('',(8.8,4.7,6.5));
#15823=CARTESIAN_POINT('',(8.8,4.7,6.5));
#15824=CARTESIAN_POINT('',(8.8,4.7,2.3));
#15825=CARTESIAN_POINT('Origin',(8.8,-4.7,2.3));
#15826=CARTESIAN_POINT('',(8.8,-4.7,2.3));
#15827=CARTESIAN_POINT('',(8.8,-4.7,2.3));
#15828=CARTESIAN_POINT('',(8.8,-4.7,6.5));
#15829=CARTESIAN_POINT('',(8.8,-4.7,6.5));
#15830=CARTESIAN_POINT('',(8.8,-4.7,2.3));
#15831=CARTESIAN_POINT('Origin',(8.5,-4.7,2.3));
#15832=CARTESIAN_POINT('',(8.5,-4.7,2.3));
#15833=CARTESIAN_POINT('',(8.5,-4.7,2.3));
#15834=CARTESIAN_POINT('',(8.5,-4.7,6.5));
#15835=CARTESIAN_POINT('',(8.5,-4.7,6.5));
#15836=CARTESIAN_POINT('',(8.5,-4.7,2.3));
#15837=CARTESIAN_POINT('Origin',(8.5,4.7,2.3));
#15838=CARTESIAN_POINT('',(8.5,4.7,2.3));
#15839=CARTESIAN_POINT('',(8.5,4.7,6.5));
#15840=CARTESIAN_POINT('Origin',(8.65,0.,6.5));
#15841=CARTESIAN_POINT('Origin',(8.65,0.,2.3));
#15842=CARTESIAN_POINT('',(0.,0.,0.));
#15843=CARTESIAN_POINT('Origin',(5.6,0.,2.7));
#15844=CARTESIAN_POINT('',(5.6,-0.0947295350922144,2.90408653846154));
#15845=CARTESIAN_POINT('',(5.6,0.0947295350922144,2.90408653846154));
#15846=CARTESIAN_POINT('Origin',(5.6,0.,4.));
#15847=CARTESIAN_POINT('',(5.6,-2.75545529808155E-17,2.925));
#15848=CARTESIAN_POINT('Origin',(5.6,0.,2.7));
#15849=CARTESIAN_POINT('Origin',(5.6,0.,2.7));
#15850=CARTESIAN_POINT('Origin',(5.,0.,2.7));
#15851=CARTESIAN_POINT('',(5.1,-2.75545529808155E-17,2.925));
#15852=CARTESIAN_POINT('Origin',(5.1,0.,2.7));
#15853=CARTESIAN_POINT('',(5.,-2.75545529808155E-17,2.925));
#15854=CARTESIAN_POINT('',(5.5,-0.0947295350922147,2.90408653846154));
#15855=CARTESIAN_POINT('',(5.,-0.0947295350922144,2.90408653846154));
#15856=CARTESIAN_POINT('',(5.5,0.0947295350922147,2.90408653846154));
#15857=CARTESIAN_POINT('Origin',(5.5,0.,2.7));
#15858=CARTESIAN_POINT('',(5.,0.0947295350922144,2.90408653846154));
#15859=CARTESIAN_POINT('Origin',(5.6,0.,5.3));
#15860=CARTESIAN_POINT('',(5.6,0.0947295350922135,5.09591346153846));
#15861=CARTESIAN_POINT('',(5.6,-1.34711147906209E-16,5.1));
#15862=CARTESIAN_POINT('Origin',(5.6,0.,4.));
#15863=CARTESIAN_POINT('',(5.6,-0.0947295350922135,5.09591346153846));
#15864=CARTESIAN_POINT('Origin',(5.6,0.,5.3));
#15865=CARTESIAN_POINT('Origin',(5.6,0.,4.));
#15866=CARTESIAN_POINT('Origin',(5.,0.,5.3));
#15867=CARTESIAN_POINT('',(5.1,-2.75545529808154E-17,5.525));
#15868=CARTESIAN_POINT('Origin',(5.1,0.,5.3));
#15869=CARTESIAN_POINT('',(5.5,-2.75545529808154E-17,5.525));
#15870=CARTESIAN_POINT('',(5.,-2.75545529808154E-17,5.525));
#15871=CARTESIAN_POINT('',(5.5,-0.0947295350922147,5.09591346153846));
#15872=CARTESIAN_POINT('Origin',(5.5,0.,5.3));
#15873=CARTESIAN_POINT('',(5.,-0.0947295350922135,5.09591346153846));
#15874=CARTESIAN_POINT('',(5.5,0.0947295350922147,5.09591346153846));
#15875=CARTESIAN_POINT('',(5.,0.0947295350922135,5.09591346153846));
#15876=CARTESIAN_POINT('Origin',(5.5,0.,5.3));
#15877=CARTESIAN_POINT('Origin',(5.5,0.,4.));
#15878=CARTESIAN_POINT('',(8.5,-1.34711147906209E-16,5.1));
#15879=CARTESIAN_POINT('Origin',(8.5,0.,4.));
#15880=CARTESIAN_POINT('',(5.5,-1.34711147906209E-16,5.1));
#15881=CARTESIAN_POINT('Origin',(5.5,0.,4.));
#15882=CARTESIAN_POINT('Origin',(5.5,0.,4.));
#15883=CARTESIAN_POINT('Origin',(5.5,0.,4.));
#15884=CARTESIAN_POINT('',(5.5,-1.95943487863577E-16,5.6));
#15885=CARTESIAN_POINT('Origin',(5.5,0.,4.));
#15886=CARTESIAN_POINT('Origin',(5.1,0.,4.));
#15887=CARTESIAN_POINT('',(5.1,-1.95943487863577E-16,5.6));
#15888=CARTESIAN_POINT('',(5.1,-1.95943487863577E-16,5.6));
#15889=CARTESIAN_POINT('Origin',(5.1,0.,4.));
#15890=CARTESIAN_POINT('Origin',(5.1,0.,4.));
#15891=CARTESIAN_POINT('',(5.1,-6.4293956955236E-17,4.525));
#15892=CARTESIAN_POINT('Origin',(5.1,0.,4.));
#15893=CARTESIAN_POINT('Origin',(5.5,0.,4.));
#15894=CARTESIAN_POINT('',(8.5,-6.4293956955236E-17,4.525));
#15895=CARTESIAN_POINT('Origin',(8.5,0.,4.));
#15896=CARTESIAN_POINT('',(5.5,-6.4293956955236E-17,4.525));
#15897=CARTESIAN_POINT('Origin',(8.5,0.,4.));
#15898=CARTESIAN_POINT('',(0.,0.,0.));
#15899=CARTESIAN_POINT('Origin',(4.7,2.5,7.8));
#15900=CARTESIAN_POINT('',(4.8,2.5,8.2));
#15901=CARTESIAN_POINT('Origin',(4.8,2.5,7.8));
#15902=CARTESIAN_POINT('',(5.2,2.5,8.2));
#15903=CARTESIAN_POINT('',(4.7,2.5,8.2));
#15904=CARTESIAN_POINT('Origin',(5.2,2.5,7.8));
#15905=CARTESIAN_POINT('Origin',(5.2,2.5,7.8));
#15906=CARTESIAN_POINT('',(5.2,2.5,8.025));
#15907=CARTESIAN_POINT('Origin',(5.2,2.5,7.8));
#15908=CARTESIAN_POINT('Origin',(4.7,-2.5,9.2));
#15909=CARTESIAN_POINT('',(4.8,-2.5,9.6));
#15910=CARTESIAN_POINT('Origin',(4.8,-2.5,9.2));
#15911=CARTESIAN_POINT('',(5.2,-2.5,9.6));
#15912=CARTESIAN_POINT('',(4.7,-2.5,9.6));
#15913=CARTESIAN_POINT('Origin',(5.2,-2.5,9.2));
#15914=CARTESIAN_POINT('Origin',(5.2,-2.5,9.2));
#15915=CARTESIAN_POINT('',(5.2,-2.5,9.425));
#15916=CARTESIAN_POINT('Origin',(5.2,-2.5,9.2));
#15917=CARTESIAN_POINT('Origin',(4.7,-2.5,7.8));
#15918=CARTESIAN_POINT('',(4.8,-2.5,8.2));
#15919=CARTESIAN_POINT('Origin',(4.8,-2.5,7.8));
#15920=CARTESIAN_POINT('',(5.2,-2.5,8.2));
#15921=CARTESIAN_POINT('',(4.7,-2.5,8.2));
#15922=CARTESIAN_POINT('Origin',(5.2,-2.5,7.8));
#15923=CARTESIAN_POINT('Origin',(5.2,-2.5,7.8));
#15924=CARTESIAN_POINT('',(5.2,-2.5,8.025));
#15925=CARTESIAN_POINT('Origin',(5.2,-2.5,7.8));
#15926=CARTESIAN_POINT('Origin',(4.7,2.5,9.2));
#15927=CARTESIAN_POINT('',(4.8,2.5,9.6));
#15928=CARTESIAN_POINT('Origin',(4.8,2.5,9.2));
#15929=CARTESIAN_POINT('',(5.2,2.5,9.6));
#15930=CARTESIAN_POINT('',(4.7,2.5,9.6));
#15931=CARTESIAN_POINT('Origin',(5.2,2.5,9.2));
#15932=CARTESIAN_POINT('Origin',(5.2,2.5,9.2));
#15933=CARTESIAN_POINT('',(5.2,2.5,9.425));
#15934=CARTESIAN_POINT('Origin',(5.2,2.5,9.2));
#15935=CARTESIAN_POINT('Origin',(4.7,2.5,7.8));
#15936=CARTESIAN_POINT('',(5.5,2.5,8.025));
#15937=CARTESIAN_POINT('',(4.7,2.5,8.025));
#15938=CARTESIAN_POINT('Origin',(5.5,2.5,7.8));
#15939=CARTESIAN_POINT('Origin',(4.7,-2.5,9.2));
#15940=CARTESIAN_POINT('',(5.5,-2.5,9.425));
#15941=CARTESIAN_POINT('',(4.7,-2.5,9.425));
#15942=CARTESIAN_POINT('Origin',(5.5,-2.5,9.2));
#15943=CARTESIAN_POINT('Origin',(4.7,-2.5,7.8));
#15944=CARTESIAN_POINT('',(5.5,-2.5,8.025));
#15945=CARTESIAN_POINT('',(4.7,-2.5,8.025));
#15946=CARTESIAN_POINT('Origin',(5.5,-2.5,7.8));
#15947=CARTESIAN_POINT('Origin',(4.7,2.5,9.2));
#15948=CARTESIAN_POINT('',(5.5,2.5,9.425));
#15949=CARTESIAN_POINT('',(4.7,2.5,9.425));
#15950=CARTESIAN_POINT('Origin',(5.5,2.5,9.2));
#15951=CARTESIAN_POINT('Origin',(5.5,4.,7.));
#15952=CARTESIAN_POINT('',(5.5,4.,7.));
#15953=CARTESIAN_POINT('',(4.8,4.,7.));
#15954=CARTESIAN_POINT('',(5.5,4.,7.));
#15955=CARTESIAN_POINT('',(4.8,4.,10.));
#15956=CARTESIAN_POINT('',(4.8,4.,7.));
#15957=CARTESIAN_POINT('',(5.5,4.,10.));
#15958=CARTESIAN_POINT('',(5.5,4.,10.));
#15959=CARTESIAN_POINT('',(5.5,4.,7.));
#15960=CARTESIAN_POINT('Origin',(5.5,-4.,7.));
#15961=CARTESIAN_POINT('',(5.5,-4.,7.));
#15962=CARTESIAN_POINT('',(5.5,-4.,7.));
#15963=CARTESIAN_POINT('',(5.5,-4.,10.));
#15964=CARTESIAN_POINT('',(5.5,-4.,10.));
#15965=CARTESIAN_POINT('',(5.5,-4.,7.));
#15966=CARTESIAN_POINT('Origin',(4.8,-4.,7.));
#15967=CARTESIAN_POINT('',(4.8,-4.,7.));
#15968=CARTESIAN_POINT('',(4.8,-4.,7.));
#15969=CARTESIAN_POINT('',(4.8,-4.,10.));
#15970=CARTESIAN_POINT('',(4.8,-4.,10.));
#15971=CARTESIAN_POINT('',(4.8,-4.,7.));
#15972=CARTESIAN_POINT('Origin',(4.8,4.,7.));
#15973=CARTESIAN_POINT('',(4.8,4.,7.));
#15974=CARTESIAN_POINT('',(4.8,4.,10.));
#15975=CARTESIAN_POINT('Origin',(5.15,0.,10.));
#15976=CARTESIAN_POINT('Origin',(5.15,0.,7.));
#15977=CARTESIAN_POINT('',(0.,0.,0.));
#15978=CARTESIAN_POINT('',(0.,0.,0.));
#15979=CARTESIAN_POINT('Origin',(0.75,1.2,0.));
#15980=CARTESIAN_POINT('',(0.885663593019381,1.2,-0.16));
#15981=CARTESIAN_POINT('',(0.885663593019381,1.2,0.16));
#15982=CARTESIAN_POINT('Origin',(0.,1.2,0.));
#15983=CARTESIAN_POINT('',(0.93,1.2,-0.16));
#15984=CARTESIAN_POINT('',(0.93,1.2,-0.16));
#15985=CARTESIAN_POINT('',(0.93,1.2,0.16));
#15986=CARTESIAN_POINT('',(0.93,1.2,0.16));
#15987=CARTESIAN_POINT('',(0.57,1.2,0.16));
#15988=CARTESIAN_POINT('Origin',(0.57,0.,0.16));
#15989=CARTESIAN_POINT('',(0.885663593019381,-1.2,0.16));
#15990=CARTESIAN_POINT('',(0.885663593019381,0.,0.16));
#15991=CARTESIAN_POINT('',(0.93,-1.2,0.16));
#15992=CARTESIAN_POINT('',(0.93,0.,0.16));
#15993=CARTESIAN_POINT('',(0.57,-1.2,0.16));
#15994=CARTESIAN_POINT('Origin',(0.75,-1.2,0.));
#15995=CARTESIAN_POINT('',(0.885663593019381,-1.2,-0.16));
#15996=CARTESIAN_POINT('Origin',(0.,-1.2,0.));
#15997=CARTESIAN_POINT('',(0.93,-1.2,-0.16));
#15998=CARTESIAN_POINT('',(0.93,-1.2,0.16));
#15999=CARTESIAN_POINT('',(0.93,-1.2,-0.16));
#16000=CARTESIAN_POINT('Origin',(0.93,0.,-0.16));
#16001=CARTESIAN_POINT('',(0.885663593019381,0.,-0.16));
#16002=CARTESIAN_POINT('',(0.93,0.,-0.16));
#16003=CARTESIAN_POINT('Origin',(0.93,0.,0.16));
#16004=CARTESIAN_POINT('Origin',(1.05,1.5,0.));
#16005=CARTESIAN_POINT('',(-1.05,1.5,-1.28587913910472E-16));
#16006=CARTESIAN_POINT('Origin',(0.,1.5,0.));
#16007=CARTESIAN_POINT('',(-0.9,1.5,-1.10218211923262E-16));
#16008=CARTESIAN_POINT('Origin',(0.,1.5,0.));
#16009=CARTESIAN_POINT('Origin',(0.,1.315,0.));
#16010=CARTESIAN_POINT('',(-1.05,1.13,-1.28587913910472E-16));
#16011=CARTESIAN_POINT('Origin',(0.,1.13,0.));
#16012=CARTESIAN_POINT('',(-1.05,1.315,-1.28587913910472E-16));
#16013=CARTESIAN_POINT('Origin',(1.,1.13,0.));
#16014=CARTESIAN_POINT('',(-1.,1.13,-1.22464679914735E-16));
#16015=CARTESIAN_POINT('Origin',(0.,1.13,0.));
#16016=CARTESIAN_POINT('Origin',(0.,1.065,0.));
#16017=CARTESIAN_POINT('',(-1.,1.,-1.22464679914735E-16));
#16018=CARTESIAN_POINT('Origin',(0.,1.,0.));
#16019=CARTESIAN_POINT('',(-1.,1.065,-1.22464679914735E-16));
#16020=CARTESIAN_POINT('Origin',(1.05,1.,0.));
#16021=CARTESIAN_POINT('',(-1.05,1.,-1.28587913910472E-16));
#16022=CARTESIAN_POINT('Origin',(0.,1.,0.));
#16023=CARTESIAN_POINT('Origin',(0.,0.,0.));
#16024=CARTESIAN_POINT('',(-1.05,-1.,-1.28587913910472E-16));
#16025=CARTESIAN_POINT('Origin',(0.,-1.,0.));
#16026=CARTESIAN_POINT('',(-1.05,0.,-1.28587913910472E-16));
#16027=CARTESIAN_POINT('Origin',(1.,-1.,0.));
#16028=CARTESIAN_POINT('',(-1.,-1.,-1.22464679914735E-16));
#16029=CARTESIAN_POINT('Origin',(0.,-1.,0.));
#16030=CARTESIAN_POINT('Origin',(0.,-1.065,0.));
#16031=CARTESIAN_POINT('',(-1.,-1.13,-1.22464679914735E-16));
#16032=CARTESIAN_POINT('Origin',(0.,-1.13,0.));
#16033=CARTESIAN_POINT('',(-1.,-1.065,-1.22464679914735E-16));
#16034=CARTESIAN_POINT('Origin',(1.05,-1.13,0.));
#16035=CARTESIAN_POINT('',(-1.05,-1.13,-1.28587913910472E-16));
#16036=CARTESIAN_POINT('Origin',(0.,-1.13,0.));
#16037=CARTESIAN_POINT('Origin',(0.,-1.315,0.));
#16038=CARTESIAN_POINT('',(-1.05,-1.5,-1.28587913910472E-16));
#16039=CARTESIAN_POINT('Origin',(0.,-1.5,0.));
#16040=CARTESIAN_POINT('',(-1.05,-1.315,-1.28587913910472E-16));
#16041=CARTESIAN_POINT('Origin',(0.9,-1.5,0.));
#16042=CARTESIAN_POINT('',(-0.9,-1.5,-1.10218211923262E-16));
#16043=CARTESIAN_POINT('Origin',(0.,-1.5,0.));
#16044=CARTESIAN_POINT('Origin',(0.,0.,0.));
#16045=CARTESIAN_POINT('',(-0.9,0.,-1.10218211923262E-16));
#16046=CARTESIAN_POINT('',(0.,0.,0.));
#16047=CARTESIAN_POINT('Origin',(0.75,1.2,0.));
#16048=CARTESIAN_POINT('',(0.880582193778639,1.2,0.16));
#16049=CARTESIAN_POINT('',(0.880582193778639,1.2,-0.16));
#16050=CARTESIAN_POINT('Origin',(0.,1.2,0.));
#16051=CARTESIAN_POINT('',(0.583459510163302,1.2,0.16));
#16052=CARTESIAN_POINT('',(0.57,1.2,0.16));
#16053=CARTESIAN_POINT('',(0.583459510163302,1.2,-0.16));
#16054=CARTESIAN_POINT('Origin',(0.,1.2,0.));
#16055=CARTESIAN_POINT('',(0.93,1.2,-0.16));
#16056=CARTESIAN_POINT('Origin',(0.93,0.,-0.16));
#16057=CARTESIAN_POINT('',(0.880582193778639,-1.2,-0.16));
#16058=CARTESIAN_POINT('',(0.880582193778639,0.,-0.16));
#16059=CARTESIAN_POINT('',(0.583459510163302,-1.2,-0.16));
#16060=CARTESIAN_POINT('',(0.583459510163302,0.,-0.16));
#16061=CARTESIAN_POINT('',(0.93,-1.2,-0.16));
#16062=CARTESIAN_POINT('Origin',(0.75,-1.2,0.));
#16063=CARTESIAN_POINT('',(0.880582193778639,-1.2,0.16));
#16064=CARTESIAN_POINT('Origin',(0.,-1.2,0.));
#16065=CARTESIAN_POINT('',(0.583459510163302,-1.2,0.16));
#16066=CARTESIAN_POINT('Origin',(0.,-1.2,0.));
#16067=CARTESIAN_POINT('',(0.57,-1.2,0.16));
#16068=CARTESIAN_POINT('Origin',(0.57,0.,0.16));
#16069=CARTESIAN_POINT('',(0.880582193778639,0.,0.16));
#16070=CARTESIAN_POINT('',(0.583459510163302,0.,0.16));
#16071=CARTESIAN_POINT('Origin',(0.895,1.35,0.));
#16072=CARTESIAN_POINT('',(-0.895,1.35,-1.09605888523688E-16));
#16073=CARTESIAN_POINT('Origin',(0.,1.35,0.));
#16074=CARTESIAN_POINT('',(-0.605,1.35,-7.40911313484149E-17));
#16075=CARTESIAN_POINT('Origin',(0.,1.35,0.));
#16076=CARTESIAN_POINT('Origin',(0.,0.,0.));
#16077=CARTESIAN_POINT('',(-0.895,-1.35,-1.09605888523688E-16));
#16078=CARTESIAN_POINT('Origin',(0.,-1.35,0.));
#16079=CARTESIAN_POINT('',(-0.895,0.,-1.09605888523688E-16));
#16080=CARTESIAN_POINT('Origin',(0.605,-1.35,0.));
#16081=CARTESIAN_POINT('',(-0.605,-1.35,-7.40911313484149E-17));
#16082=CARTESIAN_POINT('Origin',(0.,-1.35,0.));
#16083=CARTESIAN_POINT('Origin',(0.,0.,0.));
#16084=CARTESIAN_POINT('',(-0.605,0.,-7.40911313484149E-17));
#16085=CARTESIAN_POINT('',(0.,0.,0.));
#16086=CARTESIAN_POINT('',(0.,0.,0.));
#16087=CARTESIAN_POINT('',(0.,0.,0.));
#16088=CARTESIAN_POINT('Origin',(0.0866025403784439,-0.4,-0.15));
#16089=CARTESIAN_POINT('',(0.173205080756888,-0.4,0.));
#16090=CARTESIAN_POINT('',(0.0866025403784439,-0.4,-0.15));
#16091=CARTESIAN_POINT('',(0.173205080756888,-0.4,0.));
#16092=CARTESIAN_POINT('',(0.0866025403784439,-0.64,-0.15));
#16093=CARTESIAN_POINT('',(0.0866025403784439,-0.4,-0.15));
#16094=CARTESIAN_POINT('',(0.173205080756888,-0.64,0.));
#16095=CARTESIAN_POINT('',(0.173205080756888,-0.64,0.));
#16096=CARTESIAN_POINT('',(0.173205080756888,-0.4,0.));
#16097=CARTESIAN_POINT('Origin',(-0.0866025403784438,-0.4,-0.15));
#16098=CARTESIAN_POINT('',(-0.0866025403784438,-0.4,-0.15));
#16099=CARTESIAN_POINT('',(0.0866025403784439,-0.4,-0.15));
#16100=CARTESIAN_POINT('',(-0.0866025403784438,-0.64,-0.15));
#16101=CARTESIAN_POINT('',(-0.0866025403784438,-0.4,-0.15));
#16102=CARTESIAN_POINT('',(0.0866025403784439,-0.64,-0.15));
#16103=CARTESIAN_POINT('Origin',(-0.173205080756888,-0.4,-2.77555756156289E-17));
#16104=CARTESIAN_POINT('',(-0.173205080756888,-0.4,-2.12115047744981E-17));
#16105=CARTESIAN_POINT('',(-0.0866025403784438,-0.4,-0.15));
#16106=CARTESIAN_POINT('',(-0.173205080756888,-0.64,-2.77555756156289E-17));
#16107=CARTESIAN_POINT('',(-0.173205080756888,-0.4,-2.12115047744981E-17));
#16108=CARTESIAN_POINT('',(-0.0866025403784438,-0.64,-0.15));
#16109=CARTESIAN_POINT('Origin',(-0.0866025403784439,-0.4,0.15));
#16110=CARTESIAN_POINT('',(-0.0866025403784439,-0.4,0.15));
#16111=CARTESIAN_POINT('',(-0.173205080756888,-0.4,-2.12115047744981E-17));
#16112=CARTESIAN_POINT('',(-0.0866025403784439,-0.64,0.15));
#16113=CARTESIAN_POINT('',(-0.0866025403784439,-0.4,0.15));
#16114=CARTESIAN_POINT('',(-0.173205080756888,-0.64,-2.12115047744981E-17));
#16115=CARTESIAN_POINT('Origin',(0.0866025403784439,-0.4,0.15));
#16116=CARTESIAN_POINT('',(0.0866025403784439,-0.4,0.15));
#16117=CARTESIAN_POINT('',(-0.0866025403784439,-0.4,0.15));
#16118=CARTESIAN_POINT('',(0.0866025403784439,-0.64,0.15));
#16119=CARTESIAN_POINT('',(0.0866025403784439,-0.4,0.15));
#16120=CARTESIAN_POINT('',(-0.0866025403784439,-0.64,0.15));
#16121=CARTESIAN_POINT('Origin',(0.173205080756888,-0.4,0.));
#16122=CARTESIAN_POINT('',(0.0866025403784439,-0.4,0.15));
#16123=CARTESIAN_POINT('',(0.0866025403784439,-0.64,0.15));
#16124=CARTESIAN_POINT('Origin',(0.,-0.4,-2.77555756156289E-17));
#16125=CARTESIAN_POINT('Origin',(0.,-0.64,-2.77555756156289E-17));
#16126=CARTESIAN_POINT('Origin',(0.,-1.,0.));
#16127=CARTESIAN_POINT('',(-0.1954,-1.,2.39295984553393E-17));
#16128=CARTESIAN_POINT('Origin',(0.,-1.,0.));
#16129=CARTESIAN_POINT('Origin',(0.3,0.4,0.));
#16130=CARTESIAN_POINT('',(-0.3,0.4,-3.67394039744206E-17));
#16131=CARTESIAN_POINT('Origin',(0.,0.4,0.));
#16132=CARTESIAN_POINT('Origin',(0.,0.375,0.));
#16133=CARTESIAN_POINT('',(-0.35,0.35,-4.28626379701573E-17));
#16134=CARTESIAN_POINT('Origin',(0.,0.35,0.));
#16135=CARTESIAN_POINT('',(-0.325,0.375,-3.9801020972289E-17));
#16136=CARTESIAN_POINT('Origin',(0.,0.19,0.));
#16137=CARTESIAN_POINT('',(-0.35,0.03,-4.28626379701574E-17));
#16138=CARTESIAN_POINT('Origin',(0.,0.03,0.));
#16139=CARTESIAN_POINT('',(-0.35,0.19,-4.28626379701574E-17));
#16140=CARTESIAN_POINT('Origin',(0.,0.0149999999999999,0.));
#16141=CARTESIAN_POINT('',(-0.32,-3.29597460435593E-17,-3.91886975727153E-17));
#16142=CARTESIAN_POINT('Origin',(0.,0.,0.));
#16143=CARTESIAN_POINT('',(-0.335,0.0149999999999999,-4.10256677714363E-17));
#16144=CARTESIAN_POINT('Origin',(0.22,0.,0.));
#16145=CARTESIAN_POINT('',(-0.22,-6.93889390390723E-18,-2.69422295812418E-17));
#16146=CARTESIAN_POINT('Origin',(0.,0.,0.));
#16147=CARTESIAN_POINT('Origin',(0.,-0.02,0.));
#16148=CARTESIAN_POINT('',(-0.1954,-0.0492,2.39295984553393E-17));
#16149=CARTESIAN_POINT('Origin',(0.,-0.0492,0.));
#16150=CARTESIAN_POINT('',(-0.21,-0.02,-2.57175827820944E-17));
#16151=CARTESIAN_POINT('Origin',(0.,-0.8,0.));
#16152=CARTESIAN_POINT('',(-0.1954,-0.8,-2.39295984553393E-17));
#16153=CARTESIAN_POINT('',(0.,0.,0.));
#16154=CARTESIAN_POINT('',(0.,0.,0.));
#16155=CARTESIAN_POINT('Origin',(13.,0.,4.));
#16156=CARTESIAN_POINT('',(13.,-2.02066721859313E-17,4.165));
#16157=CARTESIAN_POINT('Origin',(13.,0.,4.));
#16158=CARTESIAN_POINT('',(14.5,2.02066721859313E-17,4.165));
#16159=CARTESIAN_POINT('',(13.,-2.02066721859313E-17,4.165));
#16160=CARTESIAN_POINT('Origin',(14.5,0.,4.));
#16161=CARTESIAN_POINT('Origin',(13.,0.,4.));
#16162=CARTESIAN_POINT('Origin',(-15.1,0.,4.));
#16163=CARTESIAN_POINT('',(-15.,-2.02066721859313E-17,4.165));
#16164=CARTESIAN_POINT('Origin',(-15.,0.,4.));
#16165=CARTESIAN_POINT('',(-13.4,-2.02066721859313E-17,4.165));
#16166=CARTESIAN_POINT('',(-15.1,-2.02066721859313E-17,4.165));
#16167=CARTESIAN_POINT('Origin',(-13.4,0.,4.));
#16168=CARTESIAN_POINT('Origin',(-13.4,0.,4.));
#16169=CARTESIAN_POINT('Origin',(11.,0.,4.));
#16170=CARTESIAN_POINT('',(11.,-9.79717439317882E-17,4.8));
#16171=CARTESIAN_POINT('Origin',(11.,0.,4.));
#16172=CARTESIAN_POINT('',(11.,-7.34788079488412E-17,4.6));
#16173=CARTESIAN_POINT('Origin',(11.,0.,4.));
#16174=CARTESIAN_POINT('Origin',(10.,0.,4.));
#16175=CARTESIAN_POINT('',(10.,-9.79717439317882E-17,4.8));
#16176=CARTESIAN_POINT('Origin',(10.,0.,4.));
#16177=CARTESIAN_POINT('',(10.,7.34788079488412E-17,4.6));
#16178=CARTESIAN_POINT('Origin',(10.,0.,4.));
#16179=CARTESIAN_POINT('Origin',(10.,0.,4.));
#16180=CARTESIAN_POINT('',(10.,-9.79717439317882E-17,4.8));
#16181=CARTESIAN_POINT('Origin',(-15.,0.,4.));
#16182=CARTESIAN_POINT('',(-10.,-7.34788079488412E-17,4.6));
#16183=CARTESIAN_POINT('',(-15.,-7.34788079488412E-17,4.6));
#16184=CARTESIAN_POINT('Origin',(-10.,0.,4.));
#16185=CARTESIAN_POINT('Origin',(-10.,0.,4.));
#16186=CARTESIAN_POINT('',(-10.,-9.79717439317882E-17,4.8));
#16187=CARTESIAN_POINT('Origin',(-10.,0.,4.));
#16188=CARTESIAN_POINT('Origin',(-11.,0.,4.));
#16189=CARTESIAN_POINT('',(-11.,-9.79717439317882E-17,4.8));
#16190=CARTESIAN_POINT('Origin',(-11.,0.,4.));
#16191=CARTESIAN_POINT('',(-11.,7.34788079488412E-17,4.6));
#16192=CARTESIAN_POINT('Origin',(-11.,0.,4.));
#16193=CARTESIAN_POINT('Origin',(-11.,0.,4.));
#16194=CARTESIAN_POINT('',(-11.,-9.79717439317882E-17,4.8));
#16195=CARTESIAN_POINT('Origin',(-15.,0.,4.));
#16196=CARTESIAN_POINT('',(-15.,-7.34788079488412E-17,4.6));
#16197=CARTESIAN_POINT('',(-15.,-7.34788079488412E-17,4.6));
#16198=CARTESIAN_POINT('Origin',(-15.,0.,4.));
#16199=CARTESIAN_POINT('Origin',(-15.,0.,4.));
#16200=CARTESIAN_POINT('',(14.5,-7.34788079488412E-17,4.6));
#16201=CARTESIAN_POINT('Origin',(14.5,0.,4.));
#16202=CARTESIAN_POINT('',(-15.,-7.34788079488412E-17,4.6));
#16203=CARTESIAN_POINT('Origin',(14.5,0.,4.));
#16204=CARTESIAN_POINT('Origin',(-15.,0.,4.));
#16205=CARTESIAN_POINT('',(0.,0.,0.));
#16206=CARTESIAN_POINT('Origin',(-13.5,0.,4.));
#16207=CARTESIAN_POINT('',(-12.,-7.40911313484149E-17,4.605));
#16208=CARTESIAN_POINT('Origin',(-12.,0.,4.));
#16209=CARTESIAN_POINT('',(-13.5,-7.40911313484149E-17,4.605));
#16210=CARTESIAN_POINT('',(-13.5,-7.40911313484149E-17,4.605));
#16211=CARTESIAN_POINT('Origin',(-13.5,0.,4.));
#16212=CARTESIAN_POINT('Origin',(-13.5,0.,4.));
#16213=CARTESIAN_POINT('',(-12.,-9.79717439317882E-17,4.8));
#16214=CARTESIAN_POINT('Origin',(-12.,0.,4.));
#16215=CARTESIAN_POINT('',(-13.5,-9.79717439317882E-17,4.8));
#16216=CARTESIAN_POINT('',(-13.5,-9.79717439317882E-17,4.8));
#16217=CARTESIAN_POINT('Origin',(-13.5,0.,4.));
#16218=CARTESIAN_POINT('Origin',(-12.,0.,4.));
#16219=CARTESIAN_POINT('Origin',(-13.5,0.,4.));
#16220=CARTESIAN_POINT('',(0.,0.,0.));
#16221=CARTESIAN_POINT('Origin',(12.,0.,4.));
#16222=CARTESIAN_POINT('',(13.5,-7.40911313484149E-17,4.605));
#16223=CARTESIAN_POINT('Origin',(13.5,0.,4.));
#16224=CARTESIAN_POINT('',(12.,-7.40911313484149E-17,4.605));
#16225=CARTESIAN_POINT('',(12.,-7.40911313484149E-17,4.605));
#16226=CARTESIAN_POINT('Origin',(12.,0.,4.));
#16227=CARTESIAN_POINT('Origin',(12.,0.,4.));
#16228=CARTESIAN_POINT('',(13.5,-9.79717439317882E-17,4.8));
#16229=CARTESIAN_POINT('Origin',(13.5,0.,4.));
#16230=CARTESIAN_POINT('',(12.,-9.79717439317882E-17,4.8));
#16231=CARTESIAN_POINT('',(12.,-9.79717439317882E-17,4.8));
#16232=CARTESIAN_POINT('Origin',(12.,0.,4.));
#16233=CARTESIAN_POINT('Origin',(13.5,0.,4.));
#16234=CARTESIAN_POINT('Origin',(12.,0.,4.));
#16235=CARTESIAN_POINT('',(0.,0.,0.));
#16236=CARTESIAN_POINT('Origin',(-15.1,0.,4.));
#16237=CARTESIAN_POINT('',(-15.,2.81668763803891E-16,6.3));
#16238=CARTESIAN_POINT('Origin',(-15.,0.,4.));
#16239=CARTESIAN_POINT('',(-14.4,-2.81668763803891E-16,6.3));
#16240=CARTESIAN_POINT('',(-15.1,-2.81668763803891E-16,6.3));
#16241=CARTESIAN_POINT('Origin',(-14.4,0.,4.));
#16242=CARTESIAN_POINT('Origin',(-14.,0.,4.59));
#16243=CARTESIAN_POINT('',(-14.1237941840314,-0.109087121146358,4.59));
#16244=CARTESIAN_POINT('',(-13.8762058159686,-0.109087121146358,4.59));
#16245=CARTESIAN_POINT('',(-15.,-0.109087121146358,4.59));
#16246=CARTESIAN_POINT('Origin',(-14.,0.,4.59));
#16247=CARTESIAN_POINT('Origin',(-14.,0.,4.59));
#16248=CARTESIAN_POINT('',(-14.1237941840314,0.109087121146358,4.59));
#16249=CARTESIAN_POINT('',(-14.165,1.24480690947329E-17,4.6));
#16250=CARTESIAN_POINT('Ctrl Pts',(-14.1237941840314,0.109087121146359,
4.59));
#16251=CARTESIAN_POINT('Ctrl Pts',(-14.1353991351895,0.0959175971526122,
4.59243495840567));
#16252=CARTESIAN_POINT('Ctrl Pts',(-14.1453456436582,0.080223449437719,
4.59485638705045));
#16253=CARTESIAN_POINT('Ctrl Pts',(-14.160814864634,0.04298016596019,4.59880705606552));
#16254=CARTESIAN_POINT('Ctrl Pts',(-14.165,0.0208318535088818,4.6));
#16255=CARTESIAN_POINT('Ctrl Pts',(-14.165,2.77555756156289E-17,4.6));
#16256=CARTESIAN_POINT('',(-13.8762058159686,0.109087121146358,4.59));
#16257=CARTESIAN_POINT('Origin',(-14.,0.,4.59));
#16258=CARTESIAN_POINT('',(-13.835,-8.98382835879169E-18,4.6));
#16259=CARTESIAN_POINT('Ctrl Pts',(-13.835,-2.08166817117217E-17,4.6));
#16260=CARTESIAN_POINT('Ctrl Pts',(-13.835,0.0208318535088817,4.6));
#16261=CARTESIAN_POINT('Ctrl Pts',(-13.839185135366,0.0429801659601899,
4.59880705606552));
#16262=CARTESIAN_POINT('Ctrl Pts',(-13.8546543563418,0.0802234494377183,
4.59485638705045));
#16263=CARTESIAN_POINT('Ctrl Pts',(-13.8646008648105,0.0959175971526114,
4.59243495840567));
#16264=CARTESIAN_POINT('Ctrl Pts',(-13.8762058159686,0.109087121146357,
4.59));
#16265=CARTESIAN_POINT('Ctrl Pts',(-13.8762058159686,-0.109087121146357,
4.59));
#16266=CARTESIAN_POINT('Ctrl Pts',(-13.8646008648105,-0.0959175971526111,
4.59243495840567));
#16267=CARTESIAN_POINT('Ctrl Pts',(-13.8546543563418,-0.0802234494377185,
4.59485638705045));
#16268=CARTESIAN_POINT('Ctrl Pts',(-13.839185135366,-0.0429801659601899,
4.59880705606552));
#16269=CARTESIAN_POINT('Ctrl Pts',(-13.835,-0.0208318535088816,4.6));
#16270=CARTESIAN_POINT('Ctrl Pts',(-13.835,1.31838984174237E-16,4.6));
#16271=CARTESIAN_POINT('Ctrl Pts',(-14.165,-6.93889390390723E-18,4.6));
#16272=CARTESIAN_POINT('Ctrl Pts',(-14.165,-0.0208318535088817,4.6));
#16273=CARTESIAN_POINT('Ctrl Pts',(-14.160814864634,-0.04298016596019,4.59880705606552));
#16274=CARTESIAN_POINT('Ctrl Pts',(-14.1453456436582,-0.0802234494377193,
4.59485638705045));
#16275=CARTESIAN_POINT('Ctrl Pts',(-14.1353991351895,-0.0959175971526121,
4.59243495840567));
#16276=CARTESIAN_POINT('Ctrl Pts',(-14.1237941840314,-0.109087121146359,
4.59));
#16277=CARTESIAN_POINT('',(-14.165,-2.02066721859312E-17,5.2));
#16278=CARTESIAN_POINT('',(-14.165,-2.02066721859312E-17,4.59));
#16279=CARTESIAN_POINT('',(-14.,-0.164999999999999,5.18860212013945));
#16280=CARTESIAN_POINT('Ctrl Pts',(-14.,-0.164999999999999,5.18860212013945));
#16281=CARTESIAN_POINT('Ctrl Pts',(-14.0207461436607,-0.164999999999999,
5.18860212013945));
#16282=CARTESIAN_POINT('Ctrl Pts',(-14.0428569170208,-0.160848489718829,
5.18920136323583));
#16283=CARTESIAN_POINT('Ctrl Pts',(-14.0835015842248,-0.144001521209443,
5.19135875380323));
#16284=CARTESIAN_POINT('Ctrl Pts',(-14.1020377548452,-0.131307482946398,
5.19288497691659));
#16285=CARTESIAN_POINT('Ctrl Pts',(-14.1313073033885,-0.102037934403068,
5.19574431960517));
#16286=CARTESIAN_POINT('Ctrl Pts',(-14.1440014824454,-0.0835016860163233,
5.1972642227448));
#16287=CARTESIAN_POINT('Ctrl Pts',(-14.1608485537388,-0.0428567542973034,
5.19940712405299));
#16288=CARTESIAN_POINT('Ctrl Pts',(-14.165,-0.0207458891223613,5.2));
#16289=CARTESIAN_POINT('Ctrl Pts',(-14.165,2.77555756156289E-17,5.2));
#16290=CARTESIAN_POINT('',(-13.835,-6.30704670929804E-17,5.2));
#16291=CARTESIAN_POINT('Ctrl Pts',(-13.835,3.46944695195361E-17,5.2));
#16292=CARTESIAN_POINT('Ctrl Pts',(-13.835,-0.0207458891223613,5.2));
#16293=CARTESIAN_POINT('Ctrl Pts',(-13.8391514462612,-0.0428567542973019,
5.19940712405299));
#16294=CARTESIAN_POINT('Ctrl Pts',(-13.8559985175546,-0.083501686016322,
5.1972642227448));
#16295=CARTESIAN_POINT('Ctrl Pts',(-13.8686926966115,-0.102037934403068,
5.19574431960517));
#16296=CARTESIAN_POINT('Ctrl Pts',(-13.8979622451548,-0.131307482946398,
5.19288497691659));
#16297=CARTESIAN_POINT('Ctrl Pts',(-13.9164984157752,-0.144001521209443,
5.19135875380323));
#16298=CARTESIAN_POINT('Ctrl Pts',(-13.9571430829792,-0.160848489718829,
5.18920136323583));
#16299=CARTESIAN_POINT('Ctrl Pts',(-13.9792538563393,-0.164999999999999,
5.18860212013945));
#16300=CARTESIAN_POINT('Ctrl Pts',(-14.,-0.164999999999999,5.18860212013945));
#16301=CARTESIAN_POINT('Ctrl Pts',(-14.165,2.08166817117217E-17,5.2));
#16302=CARTESIAN_POINT('Ctrl Pts',(-14.165,0.0207458891223613,5.2));
#16303=CARTESIAN_POINT('Ctrl Pts',(-14.1608485537388,0.042856754297302,
5.19940712405299));
#16304=CARTESIAN_POINT('Ctrl Pts',(-14.1440014824454,0.083501686016322,
5.1972642227448));
#16305=CARTESIAN_POINT('Ctrl Pts',(-14.1313073033885,0.102037934403068,
5.19574431960517));
#16306=CARTESIAN_POINT('Ctrl Pts',(-14.1020377548452,0.131307482946398,
5.19288497691659));
#16307=CARTESIAN_POINT('Ctrl Pts',(-14.0835015842248,0.144001521209443,
5.19135875380323));
#16308=CARTESIAN_POINT('Ctrl Pts',(-14.0428569170208,0.160848489718829,
5.18920136323583));
#16309=CARTESIAN_POINT('Ctrl Pts',(-14.0207461436607,0.164999999999999,
5.18860212013945));
#16310=CARTESIAN_POINT('Ctrl Pts',(-13.9792538563393,0.164999999999999,
5.18860212013945));
#16311=CARTESIAN_POINT('Ctrl Pts',(-13.9571430829792,0.160848489718829,
5.18920136323583));
#16312=CARTESIAN_POINT('Ctrl Pts',(-13.9164984157752,0.144001521209443,
5.19135875380323));
#16313=CARTESIAN_POINT('Ctrl Pts',(-13.8979622451548,0.131307482946398,
5.19288497691659));
#16314=CARTESIAN_POINT('Ctrl Pts',(-13.8686926966115,0.102037934403068,
5.19574431960517));
#16315=CARTESIAN_POINT('Ctrl Pts',(-13.8559985175546,0.083501686016322,
5.1972642227448));
#16316=CARTESIAN_POINT('Ctrl Pts',(-13.8391514462612,0.042856754297302,
5.19940712405299));
#16317=CARTESIAN_POINT('Ctrl Pts',(-13.835,0.0207458891223614,5.2));
#16318=CARTESIAN_POINT('Ctrl Pts',(-13.835,4.85722573273506E-17,5.2));
#16319=CARTESIAN_POINT('Origin',(-14.,0.,4.59));
#16320=CARTESIAN_POINT('',(-15.,0.109087121146358,4.59));
#16321=CARTESIAN_POINT('Origin',(-14.4,0.,4.));
#16322=CARTESIAN_POINT('',(-14.4,-1.46957615897682E-16,5.2));
#16323=CARTESIAN_POINT('Origin',(-14.4,0.,4.));
#16324=CARTESIAN_POINT('Origin',(-15.,0.,4.));
#16325=CARTESIAN_POINT('',(-13.5,-7.34788079488412E-17,4.6));
#16326=CARTESIAN_POINT('Origin',(-13.5,0.,4.));
#16327=CARTESIAN_POINT('',(-15.,-7.34788079488412E-17,4.6));
#16328=CARTESIAN_POINT('',(-15.,-7.34788079488412E-17,4.6));
#16329=CARTESIAN_POINT('',(-15.,-7.34788079488412E-17,4.6));
#16330=CARTESIAN_POINT('Origin',(-15.,0.,4.));
#16331=CARTESIAN_POINT('Origin',(-15.,0.,4.));
#16332=CARTESIAN_POINT('',(-13.5,-1.46957615897682E-16,5.2));
#16333=CARTESIAN_POINT('Origin',(-13.5,0.,4.));
#16334=CARTESIAN_POINT('',(-15.,-1.46957615897682E-16,5.2));
#16335=CARTESIAN_POINT('',(-15.,-1.46957615897682E-16,5.2));
#16336=CARTESIAN_POINT('Origin',(-13.5,0.,4.));
#16337=CARTESIAN_POINT('Origin',(-15.,0.,4.));
#16338=CARTESIAN_POINT('',(0.,0.,0.));
#16339=CARTESIAN_POINT('Origin',(-15.2,0.,4.));
#16340=CARTESIAN_POINT('',(-15.,-2.75545529808155E-17,4.225));
#16341=CARTESIAN_POINT('Origin',(-15.,0.,4.));
#16342=CARTESIAN_POINT('',(-15.2,-2.75545529808155E-17,4.225));
#16343=CARTESIAN_POINT('',(-15.2,-2.75545529808155E-17,4.225));
#16344=CARTESIAN_POINT('Origin',(-15.2,0.,4.));
#16345=CARTESIAN_POINT('Origin',(-15.2,0.,4.));
#16346=CARTESIAN_POINT('',(-15.,-1.22464679914735E-16,5.));
#16347=CARTESIAN_POINT('Origin',(-15.,0.,4.));
#16348=CARTESIAN_POINT('',(-15.2,-1.22464679914735E-16,5.));
#16349=CARTESIAN_POINT('',(-15.2,-1.22464679914735E-16,5.));
#16350=CARTESIAN_POINT('Origin',(-15.2,0.,4.));
#16351=CARTESIAN_POINT('Origin',(-15.,0.,4.));
#16352=CARTESIAN_POINT('Origin',(-15.2,0.,4.));
#16353=CARTESIAN_POINT('',(0.,0.,0.));
#16354=CARTESIAN_POINT('Origin',(14.5,0.,4.));
#16355=CARTESIAN_POINT('',(14.7,-2.75545529808155E-17,4.225));
#16356=CARTESIAN_POINT('Origin',(14.7,0.,4.));
#16357=CARTESIAN_POINT('',(14.5,-2.75545529808155E-17,4.225));
#16358=CARTESIAN_POINT('',(14.5,-2.75545529808155E-17,4.225));
#16359=CARTESIAN_POINT('Origin',(14.5,0.,4.));
#16360=CARTESIAN_POINT('Origin',(14.5,0.,4.));
#16361=CARTESIAN_POINT('',(14.7,-1.22464679914735E-16,5.));
#16362=CARTESIAN_POINT('Origin',(14.7,0.,4.));
#16363=CARTESIAN_POINT('',(14.5,-1.22464679914735E-16,5.));
#16364=CARTESIAN_POINT('',(14.5,-1.22464679914735E-16,5.));
#16365=CARTESIAN_POINT('Origin',(14.5,0.,4.));
#16366=CARTESIAN_POINT('Origin',(14.7,0.,4.));
#16367=CARTESIAN_POINT('Origin',(14.5,0.,4.));
#16368=CARTESIAN_POINT('',(0.,0.,0.));
#16369=CARTESIAN_POINT('Origin',(14.,0.,4.59));
#16370=CARTESIAN_POINT('',(13.9035634923901,-0.133884278389959,4.59));
#16371=CARTESIAN_POINT('',(14.0964365076099,-0.133884278389959,4.59));
#16372=CARTESIAN_POINT('',(13.5,-0.133884278389959,4.59));
#16373=CARTESIAN_POINT('Origin',(14.,0.,4.59));
#16374=CARTESIAN_POINT('Origin',(14.,0.,4.59));
#16375=CARTESIAN_POINT('',(13.9035634923901,0.133884278389959,4.59));
#16376=CARTESIAN_POINT('',(13.835,-8.64311690359451E-17,4.605));
#16377=CARTESIAN_POINT('Ctrl Pts',(13.9035634923901,0.133884278389959,4.59));
#16378=CARTESIAN_POINT('Ctrl Pts',(13.8962316423768,0.128603165341393,4.59119840340611));
#16379=CARTESIAN_POINT('Ctrl Pts',(13.8894472111884,0.122792448979943,4.59244064128815));
#16380=CARTESIAN_POINT('Ctrl Pts',(13.8687385941683,0.10208383195986,4.59651064111414));
#16381=CARTESIAN_POINT('Ctrl Pts',(13.8560565239921,0.0836002135946602,
4.59954409498317));
#16382=CARTESIAN_POINT('Ctrl Pts',(13.8391843843662,0.0429774150042655,
4.60381707438298));
#16383=CARTESIAN_POINT('Ctrl Pts',(13.835,0.0208299403327843,4.605));
#16384=CARTESIAN_POINT('Ctrl Pts',(13.835,1.94289029309402E-16,4.605));
#16385=CARTESIAN_POINT('',(14.0964365076099,0.133884278389959,4.59));
#16386=CARTESIAN_POINT('Origin',(14.,0.,4.59));
#16387=CARTESIAN_POINT('',(14.165,-1.96983309144393E-17,4.605));
#16388=CARTESIAN_POINT('Ctrl Pts',(14.165,3.46944695195361E-17,4.605));
#16389=CARTESIAN_POINT('Ctrl Pts',(14.165,0.0208299403327841,4.605));
#16390=CARTESIAN_POINT('Ctrl Pts',(14.1608156156338,0.0429774150042654,
4.60381707438298));
#16391=CARTESIAN_POINT('Ctrl Pts',(14.1439434760079,0.0836002135946602,
4.59954409498317));
#16392=CARTESIAN_POINT('Ctrl Pts',(14.1312614058317,0.10208383195986,4.59651064111414));
#16393=CARTESIAN_POINT('Ctrl Pts',(14.1105527888116,0.122792448979943,4.59244064128815));
#16394=CARTESIAN_POINT('Ctrl Pts',(14.1037683576232,0.128603165341394,4.59119840340611));
#16395=CARTESIAN_POINT('Ctrl Pts',(14.0964365076099,0.13388427838996,4.59));
#16396=CARTESIAN_POINT('Ctrl Pts',(14.0964365076099,-0.13388427838996,4.59));
#16397=CARTESIAN_POINT('Ctrl Pts',(14.1037683576232,-0.128603165341392,
4.59119840340611));
#16398=CARTESIAN_POINT('Ctrl Pts',(14.1105527888116,-0.122792448979944,
4.59244064128815));
#16399=CARTESIAN_POINT('Ctrl Pts',(14.1312614058317,-0.10208383195986,4.59651064111414));
#16400=CARTESIAN_POINT('Ctrl Pts',(14.1439434760079,-0.0836002135946602,
4.59954409498317));
#16401=CARTESIAN_POINT('Ctrl Pts',(14.1608156156338,-0.0429774150042654,
4.60381707438298));
#16402=CARTESIAN_POINT('Ctrl Pts',(14.165,-0.0208299403327839,4.605));
#16403=CARTESIAN_POINT('Ctrl Pts',(14.165,1.14491749414469E-16,4.605));
#16404=CARTESIAN_POINT('Ctrl Pts',(13.835,-1.52655665885959E-16,4.605));
#16405=CARTESIAN_POINT('Ctrl Pts',(13.835,-0.0208299403327842,4.605));
#16406=CARTESIAN_POINT('Ctrl Pts',(13.8391843843662,-0.0429774150042655,
4.60381707438298));
#16407=CARTESIAN_POINT('Ctrl Pts',(13.8560565239921,-0.0836002135946602,
4.59954409498317));
#16408=CARTESIAN_POINT('Ctrl Pts',(13.8687385941683,-0.10208383195986,4.59651064111414));
#16409=CARTESIAN_POINT('Ctrl Pts',(13.8894472111884,-0.122792448979943,
4.59244064128815));
#16410=CARTESIAN_POINT('Ctrl Pts',(13.8962316423768,-0.128603165341393,
4.59119840340611));
#16411=CARTESIAN_POINT('Ctrl Pts',(13.9035634923901,-0.133884278389959,
4.59));
#16412=CARTESIAN_POINT('',(13.835,-2.02066721859312E-17,5.));
#16413=CARTESIAN_POINT('',(13.835,-2.02066721859312E-17,4.59));
#16414=CARTESIAN_POINT('',(14.,-0.164999999999999,4.98629356684508));
#16415=CARTESIAN_POINT('Ctrl Pts',(14.,-0.164999999999999,4.98629356684508));
#16416=CARTESIAN_POINT('Ctrl Pts',(13.9792411222579,-0.164999999999999,
4.98629356684508));
#16417=CARTESIAN_POINT('Ctrl Pts',(13.9571250491954,-0.160843546393744,
4.98701673104451));
#16418=CARTESIAN_POINT('Ctrl Pts',(13.9164840215393,-0.143993021293681,
4.98961542163351));
#16419=CARTESIAN_POINT('Ctrl Pts',(13.8979557419361,-0.131300979727688,
4.99145196292459));
#16420=CARTESIAN_POINT('Ctrl Pts',(13.8686993953868,-0.102044633178354,
4.99488884996167));
#16421=CARTESIAN_POINT('Ctrl Pts',(13.8560070595837,-0.0835161924492572,
4.99671442041539));
#16422=CARTESIAN_POINT('Ctrl Pts',(13.8391563208071,-0.0428746115883117,
4.99928792543863));
#16423=CARTESIAN_POINT('Ctrl Pts',(13.835,-0.0207583454229728,5.));
#16424=CARTESIAN_POINT('Ctrl Pts',(13.835,4.85722573273506E-17,5.));
#16425=CARTESIAN_POINT('',(14.165,-3.34767643417387E-17,5.));
#16426=CARTESIAN_POINT('Ctrl Pts',(14.165,5.55111512312578E-17,5.));
#16427=CARTESIAN_POINT('Ctrl Pts',(14.165,-0.0207583454229728,5.));
#16428=CARTESIAN_POINT('Ctrl Pts',(14.1608436791929,-0.0428746115883117,
4.99928792543863));
#16429=CARTESIAN_POINT('Ctrl Pts',(14.1439929404163,-0.0835161924492572,
4.99671442041539));
#16430=CARTESIAN_POINT('Ctrl Pts',(14.1313006046132,-0.102044633178354,
4.99488884996167));
#16431=CARTESIAN_POINT('Ctrl Pts',(14.1020442580639,-0.131300979727688,
4.99145196292459));
#16432=CARTESIAN_POINT('Ctrl Pts',(14.0835159784607,-0.143993021293681,
4.98961542163351));
#16433=CARTESIAN_POINT('Ctrl Pts',(14.0428749508046,-0.160843546393744,
4.98701673104451));
#16434=CARTESIAN_POINT('Ctrl Pts',(14.0207588777421,-0.164999999999999,
4.98629356684508));
#16435=CARTESIAN_POINT('Ctrl Pts',(14.,-0.164999999999999,4.98629356684508));
#16436=CARTESIAN_POINT('Ctrl Pts',(13.835,-1.2490009027033E-16,5.));
#16437=CARTESIAN_POINT('Ctrl Pts',(13.835,0.0207583454229727,5.));
#16438=CARTESIAN_POINT('Ctrl Pts',(13.8391563208071,0.0428746115883117,
4.99928792543863));
#16439=CARTESIAN_POINT('Ctrl Pts',(13.8560070595837,0.0835161924492572,
4.99671442041539));
#16440=CARTESIAN_POINT('Ctrl Pts',(13.8686993953868,0.102044633178354,4.99488884996167));
#16441=CARTESIAN_POINT('Ctrl Pts',(13.8979557419361,0.131300979727688,4.99145196292459));
#16442=CARTESIAN_POINT('Ctrl Pts',(13.9164840215393,0.143993021293681,4.98961542163351));
#16443=CARTESIAN_POINT('Ctrl Pts',(13.9571250491954,0.160843546393744,4.98701673104451));
#16444=CARTESIAN_POINT('Ctrl Pts',(13.9792411222579,0.164999999999999,4.98629356684509));
#16445=CARTESIAN_POINT('Ctrl Pts',(14.0207588777421,0.164999999999999,4.98629356684509));
#16446=CARTESIAN_POINT('Ctrl Pts',(14.0428749508046,0.160843546393744,4.98701673104451));
#16447=CARTESIAN_POINT('Ctrl Pts',(14.0835159784607,0.143993021293681,4.98961542163351));
#16448=CARTESIAN_POINT('Ctrl Pts',(14.1020442580639,0.131300979727688,4.99145196292459));
#16449=CARTESIAN_POINT('Ctrl Pts',(14.1313006046132,0.102044633178354,4.99488884996167));
#16450=CARTESIAN_POINT('Ctrl Pts',(14.1439929404163,0.0835161924492573,
4.99671442041539));
#16451=CARTESIAN_POINT('Ctrl Pts',(14.1608436791929,0.0428746115883117,
4.99928792543863));
#16452=CARTESIAN_POINT('Ctrl Pts',(14.165,0.0207583454229729,5.));
#16453=CARTESIAN_POINT('Ctrl Pts',(14.165,1.45716771982052E-16,5.));
#16454=CARTESIAN_POINT('Origin',(14.,0.,4.59));
#16455=CARTESIAN_POINT('',(13.5,0.133884278389959,4.59));
#16456=CARTESIAN_POINT('Origin',(13.5,0.,4.));
#16457=CARTESIAN_POINT('',(14.5,-7.40911313484149E-17,4.605));
#16458=CARTESIAN_POINT('Origin',(14.5,0.,4.));
#16459=CARTESIAN_POINT('',(13.5,-7.40911313484149E-17,4.605));
#16460=CARTESIAN_POINT('',(13.5,-7.40911313484149E-17,4.605));
#16461=CARTESIAN_POINT('',(13.5,-7.40911313484149E-17,4.605));
#16462=CARTESIAN_POINT('Origin',(13.5,0.,4.));
#16463=CARTESIAN_POINT('Origin',(13.5,0.,4.));
#16464=CARTESIAN_POINT('',(14.5,-1.22464679914735E-16,5.));
#16465=CARTESIAN_POINT('Origin',(14.5,0.,4.));
#16466=CARTESIAN_POINT('',(13.5,-1.22464679914735E-16,5.));
#16467=CARTESIAN_POINT('',(13.5,-1.22464679914735E-16,5.));
#16468=CARTESIAN_POINT('',(13.5,-1.22464679914735E-16,5.));
#16469=CARTESIAN_POINT('Origin',(13.5,0.,4.));
#16470=CARTESIAN_POINT('Origin',(14.5,0.,4.));
#16471=CARTESIAN_POINT('Origin',(13.5,0.,4.));
#16472=CARTESIAN_POINT('',(0.,0.,0.));
#16473=CARTESIAN_POINT('Origin',(0.3,0.4,0.));
#16474=CARTESIAN_POINT('',(-0.3,0.4,-3.67394039744206E-17));
#16475=CARTESIAN_POINT('Origin',(0.,0.4,0.));
#16476=CARTESIAN_POINT('Origin',(0.,0.375,0.));
#16477=CARTESIAN_POINT('',(-0.35,0.35,-4.28626379701573E-17));
#16478=CARTESIAN_POINT('Origin',(0.,0.35,0.));
#16479=CARTESIAN_POINT('',(-0.325,0.375,-3.9801020972289E-17));
#16480=CARTESIAN_POINT('Origin',(0.,0.19,0.));
#16481=CARTESIAN_POINT('',(-0.35,0.03,-4.28626379701574E-17));
#16482=CARTESIAN_POINT('Origin',(0.,0.03,0.));
#16483=CARTESIAN_POINT('',(-0.35,0.19,-4.28626379701574E-17));
#16484=CARTESIAN_POINT('Origin',(0.,0.0149999999999999,0.));
#16485=CARTESIAN_POINT('',(-0.32,-3.29597460435593E-17,-3.91886975727153E-17));
#16486=CARTESIAN_POINT('Origin',(0.,0.,0.));
#16487=CARTESIAN_POINT('',(-0.335,0.0149999999999999,-4.10256677714363E-17));
#16488=CARTESIAN_POINT('Origin',(0.22,0.,0.));
#16489=CARTESIAN_POINT('',(-0.22,-6.93889390390723E-18,-2.69422295812418E-17));
#16490=CARTESIAN_POINT('Origin',(0.,0.,0.));
#16491=CARTESIAN_POINT('Origin',(0.,-0.02,0.));
#16492=CARTESIAN_POINT('',(-0.1954,-0.0492,2.39295984553393E-17));
#16493=CARTESIAN_POINT('Origin',(0.,-0.0492,0.));
#16494=CARTESIAN_POINT('',(-0.21,-0.02,-2.57175827820944E-17));
#16495=CARTESIAN_POINT('Origin',(0.,-0.8,0.));
#16496=CARTESIAN_POINT('',(-0.1954,-1.5646,2.39295984553393E-17));
#16497=CARTESIAN_POINT('Origin',(0.,-1.5646,0.));
#16498=CARTESIAN_POINT('',(-0.1954,-0.8,-2.39295984553393E-17));
#16499=CARTESIAN_POINT('Origin',(0.,-1.58,0.));
#16500=CARTESIAN_POINT('',(-0.16,-1.6,-1.95943487863577E-17));
#16501=CARTESIAN_POINT('Origin',(0.,-1.6,0.));
#16502=CARTESIAN_POINT('',(-0.18,-1.58,-2.20436423846524E-17));
#16503=CARTESIAN_POINT('Origin',(0.,-1.6,0.));
#16504=CARTESIAN_POINT('Origin',(0.0866025403784439,-0.4,-0.15));
#16505=CARTESIAN_POINT('',(0.173205080756888,-0.4,0.));
#16506=CARTESIAN_POINT('',(0.0866025403784439,-0.4,-0.15));
#16507=CARTESIAN_POINT('',(0.173205080756888,-0.4,0.));
#16508=CARTESIAN_POINT('',(0.0866025403784439,-0.64,-0.15));
#16509=CARTESIAN_POINT('',(0.0866025403784439,-0.4,-0.15));
#16510=CARTESIAN_POINT('',(0.173205080756888,-0.64,0.));
#16511=CARTESIAN_POINT('',(0.173205080756888,-0.64,0.));
#16512=CARTESIAN_POINT('',(0.173205080756888,-0.4,0.));
#16513=CARTESIAN_POINT('Origin',(-0.0866025403784438,-0.4,-0.15));
#16514=CARTESIAN_POINT('',(-0.0866025403784438,-0.4,-0.15));
#16515=CARTESIAN_POINT('',(0.0866025403784439,-0.4,-0.15));
#16516=CARTESIAN_POINT('',(-0.0866025403784438,-0.64,-0.15));
#16517=CARTESIAN_POINT('',(-0.0866025403784438,-0.4,-0.15));
#16518=CARTESIAN_POINT('',(0.0866025403784439,-0.64,-0.15));
#16519=CARTESIAN_POINT('Origin',(-0.173205080756888,-0.4,-2.77555756156289E-17));
#16520=CARTESIAN_POINT('',(-0.173205080756888,-0.4,-2.12115047744981E-17));
#16521=CARTESIAN_POINT('',(-0.0866025403784438,-0.4,-0.15));
#16522=CARTESIAN_POINT('',(-0.173205080756888,-0.64,-2.77555756156289E-17));
#16523=CARTESIAN_POINT('',(-0.173205080756888,-0.4,-2.12115047744981E-17));
#16524=CARTESIAN_POINT('',(-0.0866025403784438,-0.64,-0.15));
#16525=CARTESIAN_POINT('Origin',(-0.0866025403784439,-0.4,0.15));
#16526=CARTESIAN_POINT('',(-0.0866025403784439,-0.4,0.15));
#16527=CARTESIAN_POINT('',(-0.173205080756888,-0.4,-2.12115047744981E-17));
#16528=CARTESIAN_POINT('',(-0.0866025403784439,-0.64,0.15));
#16529=CARTESIAN_POINT('',(-0.0866025403784439,-0.4,0.15));
#16530=CARTESIAN_POINT('',(-0.173205080756888,-0.64,-2.12115047744981E-17));
#16531=CARTESIAN_POINT('Origin',(0.0866025403784439,-0.4,0.15));
#16532=CARTESIAN_POINT('',(0.0866025403784439,-0.4,0.15));
#16533=CARTESIAN_POINT('',(-0.0866025403784439,-0.4,0.15));
#16534=CARTESIAN_POINT('',(0.0866025403784439,-0.64,0.15));
#16535=CARTESIAN_POINT('',(0.0866025403784439,-0.4,0.15));
#16536=CARTESIAN_POINT('',(-0.0866025403784439,-0.64,0.15));
#16537=CARTESIAN_POINT('Origin',(0.173205080756888,-0.4,0.));
#16538=CARTESIAN_POINT('',(0.0866025403784439,-0.4,0.15));
#16539=CARTESIAN_POINT('',(0.0866025403784439,-0.64,0.15));
#16540=CARTESIAN_POINT('Origin',(0.,-0.4,-2.77555756156289E-17));
#16541=CARTESIAN_POINT('Origin',(0.,-0.64,-2.77555756156289E-17));
#16542=CARTESIAN_POINT('',(0.,0.,0.));
#16543=CARTESIAN_POINT('',(0.,0.,0.));
#16544=CARTESIAN_POINT('',(0.,0.,0.));
#16545=CARTESIAN_POINT('',(0.,0.,0.));
#16546=CARTESIAN_POINT('',(0.,0.,0.));
#16547=CARTESIAN_POINT('',(-7.,-3.,4.));
#16548=CARTESIAN_POINT('',(-7.,3.,4.));
#16549=CARTESIAN_POINT('',(-8.8,-4.2,3.));
#16550=CARTESIAN_POINT('',(-8.8,-4.2,5.8));
#16551=CARTESIAN_POINT('',(-8.8,4.2,3.));
#16552=CARTESIAN_POINT('',(-8.8,4.2,5.8));
#16553=CARTESIAN_POINT('',(-5.2,-4.2,3.));
#16554=CARTESIAN_POINT('',(-5.2,-4.2,5.8));
#16555=CARTESIAN_POINT('',(-5.2,4.2,3.));
#16556=CARTESIAN_POINT('',(-5.2,4.2,5.8));
#16557=CARTESIAN_POINT('',(-5.1,2.22044604925031E-16,2.7));
#16558=CARTESIAN_POINT('',(-5.1,2.22044604925031E-16,5.3));
#16559=CARTESIAN_POINT('',(-5.2,-2.5,7.8));
#16560=CARTESIAN_POINT('',(-5.2,-2.5,9.2));
#16561=CARTESIAN_POINT('',(-5.2,2.5,7.8));
#16562=CARTESIAN_POINT('',(-5.2,2.5,9.2));
#16563=CARTESIAN_POINT('',(0.,0.,0.));
#16564=CARTESIAN_POINT('',(0.,0.,0.));
#16565=CARTESIAN_POINT('',(0.,0.,0.));
#16566=CARTESIAN_POINT('',(0.,0.,0.));
#16567=CARTESIAN_POINT('',(0.,0.,0.));
#16568=CARTESIAN_POINT('',(7.,-3.,4.));
#16569=CARTESIAN_POINT('',(7.,3.,4.));
#16570=CARTESIAN_POINT('',(5.2,-4.2,3.));
#16571=CARTESIAN_POINT('',(5.2,-4.2,5.8));
#16572=CARTESIAN_POINT('',(5.2,4.2,3.));
#16573=CARTESIAN_POINT('',(5.2,4.2,5.8));
#16574=CARTESIAN_POINT('',(8.8,-4.2,3.));
#16575=CARTESIAN_POINT('',(8.8,-4.2,5.8));
#16576=CARTESIAN_POINT('',(8.8,4.2,3.));
#16577=CARTESIAN_POINT('',(8.8,4.2,5.8));
#16578=CARTESIAN_POINT('',(5.1,0.,2.7));
#16579=CARTESIAN_POINT('',(5.1,0.,5.3));
#16580=CARTESIAN_POINT('',(5.2,-2.5,7.8));
#16581=CARTESIAN_POINT('',(5.2,-2.5,9.2));
#16582=CARTESIAN_POINT('',(5.2,2.5,7.8));
#16583=CARTESIAN_POINT('',(5.2,2.5,9.2));
#16584=CARTESIAN_POINT('',(0.,0.,0.));
#16585=CARTESIAN_POINT('Origin',(0.0577350269189626,0.,-0.1));
#16586=CARTESIAN_POINT('',(0.0577350269189626,0.,-0.1));
#16587=CARTESIAN_POINT('',(0.115470053837925,0.,0.));
#16588=CARTESIAN_POINT('',(0.0934187836487032,0.,-0.0381939203391614));
#16589=CARTESIAN_POINT('',(0.0577350269189626,-0.2,-0.1));
#16590=CARTESIAN_POINT('',(0.0577350269189626,0.,-0.1));
#16591=CARTESIAN_POINT('',(0.115470053837925,-0.2,0.));
#16592=CARTESIAN_POINT('',(0.115470053837925,-0.2,0.));
#16593=CARTESIAN_POINT('',(0.115470053837925,0.,0.));
#16594=CARTESIAN_POINT('Origin',(-0.0577350269189626,0.,-0.1));
#16595=CARTESIAN_POINT('',(-0.0577350269189626,0.,-0.1));
#16596=CARTESIAN_POINT('',(0.0561324865405187,0.,-0.1));
#16597=CARTESIAN_POINT('',(-0.0577350269189626,-0.2,-0.1));
#16598=CARTESIAN_POINT('',(-0.0577350269189626,0.,-0.1));
#16599=CARTESIAN_POINT('',(0.0577350269189626,-0.2,-0.1));
#16600=CARTESIAN_POINT('Origin',(-0.115470053837925,0.,-1.38777878078145E-17));
#16601=CARTESIAN_POINT('',(-0.115470053837925,0.,-1.41410031829988E-17));
#16602=CARTESIAN_POINT('',(-0.0797862971081845,0.,-0.0618060796608387));
#16603=CARTESIAN_POINT('',(-0.115470053837925,-0.2,-1.38777878078145E-17));
#16604=CARTESIAN_POINT('',(-0.115470053837925,0.,-1.41410031829988E-17));
#16605=CARTESIAN_POINT('',(-0.0577350269189626,-0.2,-0.1));
#16606=CARTESIAN_POINT('Origin',(-0.0577350269189626,0.,0.1));
#16607=CARTESIAN_POINT('',(-0.0577350269189626,0.,0.1));
#16608=CARTESIAN_POINT('',(-0.0509187836487033,0.,0.111806079660839));
#16609=CARTESIAN_POINT('',(-0.0577350269189626,-0.2,0.1));
#16610=CARTESIAN_POINT('',(-0.0577350269189626,0.,0.1));
#16611=CARTESIAN_POINT('',(-0.115470053837925,-0.2,-1.41410031829988E-17));
#16612=CARTESIAN_POINT('Origin',(0.0577350269189626,0.,0.1));
#16613=CARTESIAN_POINT('',(0.0577350269189626,0.,0.1));
#16614=CARTESIAN_POINT('',(0.113867513459481,0.,0.1));
#16615=CARTESIAN_POINT('',(0.0577350269189626,-0.2,0.1));
#16616=CARTESIAN_POINT('',(0.0577350269189626,0.,0.1));
#16617=CARTESIAN_POINT('',(-0.0577350269189626,-0.2,0.1));
#16618=CARTESIAN_POINT('Origin',(0.115470053837925,0.,0.));
#16619=CARTESIAN_POINT('',(0.122286297108185,0.,-0.0118060796608386));
#16620=CARTESIAN_POINT('',(0.0577350269189626,-0.2,0.1));
#16621=CARTESIAN_POINT('Origin',(0.,-0.2,0.));
#16622=CARTESIAN_POINT('Origin',(0.17,0.,0.));
#16623=CARTESIAN_POINT('',(-0.17,-8.67361737988404E-18,-2.0818995585505E-17));
#16624=CARTESIAN_POINT('Origin',(0.,0.,0.));
#16625=CARTESIAN_POINT('Origin',(0.,-0.015,0.));
#16626=CARTESIAN_POINT('',(-0.1954,-0.0254,-2.39295984553393E-17));
#16627=CARTESIAN_POINT('Origin',(0.,-0.0254,0.));
#16628=CARTESIAN_POINT('',(-0.185,-0.015,-2.2655965784226E-17));
#16629=CARTESIAN_POINT('Origin',(0.,-0.2775,0.));
#16630=CARTESIAN_POINT('',(-0.1954,-0.5296,2.39295984553393E-17));
#16631=CARTESIAN_POINT('Origin',(0.,-0.5296,0.));
#16632=CARTESIAN_POINT('',(-0.1954,-0.2775,-2.39295984553393E-17));
#16633=CARTESIAN_POINT('Origin',(0.,-0.5625,0.));
#16634=CARTESIAN_POINT('',(-0.125,-0.6,-1.53080849893419E-17));
#16635=CARTESIAN_POINT('Origin',(0.,-0.6,0.));
#16636=CARTESIAN_POINT('',(-0.1625,-0.5625,-1.99005104861445E-17));
#16637=CARTESIAN_POINT('Origin',(0.,-0.6,0.));
#16638=CARTESIAN_POINT('',(0.,0.,0.));
#16639=CARTESIAN_POINT('',(0.,0.,0.));
#16640=CARTESIAN_POINT('',(0.,0.,0.));
#16641=CARTESIAN_POINT('',(0.,0.,0.));
#16642=CARTESIAN_POINT('',(0.,0.,0.));
#16643=CARTESIAN_POINT('',(0.,0.,0.));
#16644=CARTESIAN_POINT('',(0.,0.,0.));
#16645=CARTESIAN_POINT('',(0.,0.,0.));
#16646=CARTESIAN_POINT('',(0.,0.,0.));
#16647=CARTESIAN_POINT('',(0.,0.,0.));
#16648=CARTESIAN_POINT('',(0.,0.,0.));
#16649=CARTESIAN_POINT('',(0.,0.,0.));
#16650=CARTESIAN_POINT('',(0.,0.,0.));
#16651=CARTESIAN_POINT('',(-15.,-3.,4.));
#16652=CARTESIAN_POINT('',(-13.5,-4.1,2.));
#16653=CARTESIAN_POINT('',(-13.5,-1.9,2.));
#16654=CARTESIAN_POINT('',(-13.5,-3.,5.2));
#16655=CARTESIAN_POINT('',(13.5,-4.1,2.));
#16656=CARTESIAN_POINT('',(13.5,-1.9,2.));
#16657=CARTESIAN_POINT('',(13.5,-3.,5.2));
#16658=CARTESIAN_POINT('',(-15.,3.,4.));
#16659=CARTESIAN_POINT('',(-13.5,1.9,2.));
#16660=CARTESIAN_POINT('',(-13.5,4.1,2.));
#16661=CARTESIAN_POINT('',(-13.5,3.,5.2));
#16662=CARTESIAN_POINT('',(13.5,1.9,2.));
#16663=CARTESIAN_POINT('',(13.5,4.1,2.));
#16664=CARTESIAN_POINT('',(13.5,3.,5.2));
#16665=CARTESIAN_POINT('',(-11.5,-3.,1.8));
#16666=CARTESIAN_POINT('',(-11.5,3.,1.8));
#16667=CARTESIAN_POINT('',(-11.5,0.,4.));
#16668=CARTESIAN_POINT('',(-12.5,1.4142135623731,5.41421356237309));
#16669=CARTESIAN_POINT('',(-12.5,-1.41421356237309,5.41421356237309));
#16670=CARTESIAN_POINT('',(-12.5,-1.4142135623731,2.58578643762691));
#16671=CARTESIAN_POINT('',(-12.5,1.41421356237309,2.5857864376269));
#16672=CARTESIAN_POINT('',(-10.5,1.4142135623731,5.41421356237309));
#16673=CARTESIAN_POINT('',(-10.5,-1.41421356237309,5.41421356237309));
#16674=CARTESIAN_POINT('',(-10.5,-1.4142135623731,2.58578643762691));
#16675=CARTESIAN_POINT('',(-10.5,1.41421356237309,2.5857864376269));
#16676=CARTESIAN_POINT('',(11.5,-3.,1.8));
#16677=CARTESIAN_POINT('',(11.5,3.,1.8));
#16678=CARTESIAN_POINT('',(11.5,0.,4.));
#16679=CARTESIAN_POINT('',(10.5,1.4142135623731,5.41421356237309));
#16680=CARTESIAN_POINT('',(10.5,-1.41421356237309,5.41421356237309));
#16681=CARTESIAN_POINT('',(10.5,-1.4142135623731,2.58578643762691));
#16682=CARTESIAN_POINT('',(10.5,1.41421356237309,2.5857864376269));
#16683=CARTESIAN_POINT('',(12.5,1.4142135623731,5.41421356237309));
#16684=CARTESIAN_POINT('',(12.5,-1.41421356237309,5.41421356237309));
#16685=CARTESIAN_POINT('',(12.5,-1.4142135623731,2.58578643762691));
#16686=CARTESIAN_POINT('',(12.5,1.41421356237309,2.5857864376269));
#16687=CARTESIAN_POINT('',(0.,0.,0.));
#16688=CARTESIAN_POINT('',(0.,0.,0.));
#16689=CARTESIAN_POINT('',(0.,0.,0.));
#16690=CARTESIAN_POINT('',(0.,0.,0.));
#16691=CARTESIAN_POINT('',(0.,0.,0.));
#16692=CARTESIAN_POINT('',(0.,0.,0.));
#16693=CARTESIAN_POINT('',(0.,0.,0.));
#16694=CARTESIAN_POINT('',(-14.,0.,5.2));
#16695=CARTESIAN_POINT('',(-15.2,0.,4.));
#16696=CARTESIAN_POINT('',(14.7,0.,4.));
#16697=CARTESIAN_POINT('',(14.,0.,5.2));
#16698=CARTESIAN_POINT('',(0.,0.,0.));
#16699=CARTESIAN_POINT('',(0.,0.,0.));
#16700=CARTESIAN_POINT('',(0.,0.,0.));
#16701=CARTESIAN_POINT('',(0.,0.,0.));
#16702=UNCERTAINTY_MEASURE_WITH_UNIT(LENGTH_MEASURE(0.001),#16800,
'DISTANCE_ACCURACY_VALUE',
'Maximum model space distance between geometric entities at asserted c
onnectivities');
#16703=UNCERTAINTY_MEASURE_WITH_UNIT(LENGTH_MEASURE(0.001),#16800,
'DISTANCE_ACCURACY_VALUE',
'Maximum model space distance between geometric entities at asserted c
onnectivities');
#16704=UNCERTAINTY_MEASURE_WITH_UNIT(LENGTH_MEASURE(0.001),#16800,
'DISTANCE_ACCURACY_VALUE',
'Maximum model space distance between geometric entities at asserted c
onnectivities');
#16705=UNCERTAINTY_MEASURE_WITH_UNIT(LENGTH_MEASURE(0.001),#16800,
'DISTANCE_ACCURACY_VALUE',
'Maximum model space distance between geometric entities at asserted c
onnectivities');
#16706=UNCERTAINTY_MEASURE_WITH_UNIT(LENGTH_MEASURE(0.001),#16800,
'DISTANCE_ACCURACY_VALUE',
'Maximum model space distance between geometric entities at asserted c
onnectivities');
#16707=UNCERTAINTY_MEASURE_WITH_UNIT(LENGTH_MEASURE(0.001),#16800,
'DISTANCE_ACCURACY_VALUE',
'Maximum model space distance between geometric entities at asserted c
onnectivities');
#16708=UNCERTAINTY_MEASURE_WITH_UNIT(LENGTH_MEASURE(0.001),#16800,
'DISTANCE_ACCURACY_VALUE',
'Maximum model space distance between geometric entities at asserted c
onnectivities');
#16709=UNCERTAINTY_MEASURE_WITH_UNIT(LENGTH_MEASURE(0.001),#16800,
'DISTANCE_ACCURACY_VALUE',
'Maximum model space distance between geometric entities at asserted c
onnectivities');
#16710=UNCERTAINTY_MEASURE_WITH_UNIT(LENGTH_MEASURE(0.001),#16800,
'DISTANCE_ACCURACY_VALUE',
'Maximum model space distance between geometric entities at asserted c
onnectivities');
#16711=UNCERTAINTY_MEASURE_WITH_UNIT(LENGTH_MEASURE(0.001),#16800,
'DISTANCE_ACCURACY_VALUE',
'Maximum model space distance between geometric entities at asserted c
onnectivities');
#16712=UNCERTAINTY_MEASURE_WITH_UNIT(LENGTH_MEASURE(0.001),#16800,
'DISTANCE_ACCURACY_VALUE',
'Maximum model space distance between geometric entities at asserted c
onnectivities');
#16713=UNCERTAINTY_MEASURE_WITH_UNIT(LENGTH_MEASURE(0.001),#16800,
'DISTANCE_ACCURACY_VALUE',
'Maximum model space distance between geometric entities at asserted c
onnectivities');
#16714=UNCERTAINTY_MEASURE_WITH_UNIT(LENGTH_MEASURE(0.001),#16800,
'DISTANCE_ACCURACY_VALUE',
'Maximum model space distance between geometric entities at asserted c
onnectivities');
#16715=UNCERTAINTY_MEASURE_WITH_UNIT(LENGTH_MEASURE(0.001),#16800,
'DISTANCE_ACCURACY_VALUE',
'Maximum model space distance between geometric entities at asserted c
onnectivities');
#16716=UNCERTAINTY_MEASURE_WITH_UNIT(LENGTH_MEASURE(0.001),#16800,
'DISTANCE_ACCURACY_VALUE',
'Maximum model space distance between geometric entities at asserted c
onnectivities');
#16717=UNCERTAINTY_MEASURE_WITH_UNIT(LENGTH_MEASURE(0.001),#16800,
'DISTANCE_ACCURACY_VALUE',
'Maximum model space distance between geometric entities at asserted c
onnectivities');
#16718=UNCERTAINTY_MEASURE_WITH_UNIT(LENGTH_MEASURE(0.001),#16800,
'DISTANCE_ACCURACY_VALUE',
'Maximum model space distance between geometric entities at asserted c
onnectivities');
#16719=UNCERTAINTY_MEASURE_WITH_UNIT(LENGTH_MEASURE(0.001),#16800,
'DISTANCE_ACCURACY_VALUE',
'Maximum model space distance between geometric entities at asserted c
onnectivities');
#16720=UNCERTAINTY_MEASURE_WITH_UNIT(LENGTH_MEASURE(0.001),#16800,
'DISTANCE_ACCURACY_VALUE',
'Maximum model space distance between geometric entities at asserted c
onnectivities');
#16721=UNCERTAINTY_MEASURE_WITH_UNIT(LENGTH_MEASURE(0.001),#16800,
'DISTANCE_ACCURACY_VALUE',
'Maximum model space distance between geometric entities at asserted c
onnectivities');
#16722=UNCERTAINTY_MEASURE_WITH_UNIT(LENGTH_MEASURE(0.001),#16800,
'DISTANCE_ACCURACY_VALUE',
'Maximum model space distance between geometric entities at asserted c
onnectivities');
#16723=UNCERTAINTY_MEASURE_WITH_UNIT(LENGTH_MEASURE(0.001),#16800,
'DISTANCE_ACCURACY_VALUE',
'Maximum model space distance between geometric entities at asserted c
onnectivities');
#16724=UNCERTAINTY_MEASURE_WITH_UNIT(LENGTH_MEASURE(0.001),#16800,
'DISTANCE_ACCURACY_VALUE',
'Maximum model space distance between geometric entities at asserted c
onnectivities');
#16725=UNCERTAINTY_MEASURE_WITH_UNIT(LENGTH_MEASURE(0.001),#16800,
'DISTANCE_ACCURACY_VALUE',
'Maximum model space distance between geometric entities at asserted c
onnectivities');
#16726=UNCERTAINTY_MEASURE_WITH_UNIT(LENGTH_MEASURE(0.001),#16800,
'DISTANCE_ACCURACY_VALUE',
'Maximum model space distance between geometric entities at asserted c
onnectivities');
#16727=UNCERTAINTY_MEASURE_WITH_UNIT(LENGTH_MEASURE(0.001),#16800,
'DISTANCE_ACCURACY_VALUE',
'Maximum model space distance between geometric entities at asserted c
onnectivities');
#16728=UNCERTAINTY_MEASURE_WITH_UNIT(LENGTH_MEASURE(0.001),#16800,
'DISTANCE_ACCURACY_VALUE',
'Maximum model space distance between geometric entities at asserted c
onnectivities');
#16729=UNCERTAINTY_MEASURE_WITH_UNIT(LENGTH_MEASURE(0.001),#16800,
'DISTANCE_ACCURACY_VALUE',
'Maximum model space distance between geometric entities at asserted c
onnectivities');
#16730=UNCERTAINTY_MEASURE_WITH_UNIT(LENGTH_MEASURE(0.001),#16800,
'DISTANCE_ACCURACY_VALUE',
'Maximum model space distance between geometric entities at asserted c
onnectivities');
#16731=UNCERTAINTY_MEASURE_WITH_UNIT(LENGTH_MEASURE(0.001),#16800,
'DISTANCE_ACCURACY_VALUE',
'Maximum model space distance between geometric entities at asserted c
onnectivities');
#16732=UNCERTAINTY_MEASURE_WITH_UNIT(LENGTH_MEASURE(0.001),#16800,
'DISTANCE_ACCURACY_VALUE',
'Maximum model space distance between geometric entities at asserted c
onnectivities');
#16733=UNCERTAINTY_MEASURE_WITH_UNIT(LENGTH_MEASURE(0.001),#16800,
'DISTANCE_ACCURACY_VALUE',
'Maximum model space distance between geometric entities at asserted c
onnectivities');
#16734=UNCERTAINTY_MEASURE_WITH_UNIT(LENGTH_MEASURE(0.001),#16800,
'DISTANCE_ACCURACY_VALUE',
'Maximum model space distance between geometric entities at asserted c
onnectivities');
#16735=UNCERTAINTY_MEASURE_WITH_UNIT(LENGTH_MEASURE(0.001),#16800,
'DISTANCE_ACCURACY_VALUE',
'Maximum model space distance between geometric entities at asserted c
onnectivities');
#16736=UNCERTAINTY_MEASURE_WITH_UNIT(LENGTH_MEASURE(0.001),#16800,
'DISTANCE_ACCURACY_VALUE',
'Maximum model space distance between geometric entities at asserted c
onnectivities');
#16737=UNCERTAINTY_MEASURE_WITH_UNIT(LENGTH_MEASURE(0.001),#16800,
'DISTANCE_ACCURACY_VALUE',
'Maximum model space distance between geometric entities at asserted c
onnectivities');
#16738=UNCERTAINTY_MEASURE_WITH_UNIT(LENGTH_MEASURE(0.001),#16800,
'DISTANCE_ACCURACY_VALUE',
'Maximum model space distance between geometric entities at asserted c
onnectivities');
#16739=UNCERTAINTY_MEASURE_WITH_UNIT(LENGTH_MEASURE(0.001),#16800,
'DISTANCE_ACCURACY_VALUE',
'Maximum model space distance between geometric entities at asserted c
onnectivities');
#16740=UNCERTAINTY_MEASURE_WITH_UNIT(LENGTH_MEASURE(0.001),#16800,
'DISTANCE_ACCURACY_VALUE',
'Maximum model space distance between geometric entities at asserted c
onnectivities');
#16741=UNCERTAINTY_MEASURE_WITH_UNIT(LENGTH_MEASURE(0.001),#16800,
'DISTANCE_ACCURACY_VALUE',
'Maximum model space distance between geometric entities at asserted c
onnectivities');
#16742=UNCERTAINTY_MEASURE_WITH_UNIT(LENGTH_MEASURE(0.001),#16800,
'DISTANCE_ACCURACY_VALUE',
'Maximum model space distance between geometric entities at asserted c
onnectivities');
#16743=UNCERTAINTY_MEASURE_WITH_UNIT(LENGTH_MEASURE(0.001),#16800,
'DISTANCE_ACCURACY_VALUE',
'Maximum model space distance between geometric entities at asserted c
onnectivities');
#16744=UNCERTAINTY_MEASURE_WITH_UNIT(LENGTH_MEASURE(0.001),#16800,
'DISTANCE_ACCURACY_VALUE',
'Maximum model space distance between geometric entities at asserted c
onnectivities');
#16745=UNCERTAINTY_MEASURE_WITH_UNIT(LENGTH_MEASURE(0.001),#16800,
'DISTANCE_ACCURACY_VALUE',
'Maximum model space distance between geometric entities at asserted c
onnectivities');
#16746=UNCERTAINTY_MEASURE_WITH_UNIT(LENGTH_MEASURE(0.001),#16800,
'DISTANCE_ACCURACY_VALUE',
'Maximum model space distance between geometric entities at asserted c
onnectivities');
#16747=UNCERTAINTY_MEASURE_WITH_UNIT(LENGTH_MEASURE(0.001),#16800,
'DISTANCE_ACCURACY_VALUE',
'Maximum model space distance between geometric entities at asserted c
onnectivities');
#16748=UNCERTAINTY_MEASURE_WITH_UNIT(LENGTH_MEASURE(0.001),#16800,
'DISTANCE_ACCURACY_VALUE',
'Maximum model space distance between geometric entities at asserted c
onnectivities');
#16749=UNCERTAINTY_MEASURE_WITH_UNIT(LENGTH_MEASURE(0.001),#16800,
'DISTANCE_ACCURACY_VALUE',
'Maximum model space distance between geometric entities at asserted c
onnectivities');
#16750=UNCERTAINTY_MEASURE_WITH_UNIT(LENGTH_MEASURE(0.001),#16800,
'DISTANCE_ACCURACY_VALUE',
'Maximum model space distance between geometric entities at asserted c
onnectivities');
#16751=(
GEOMETRIC_REPRESENTATION_CONTEXT(3)
GLOBAL_UNCERTAINTY_ASSIGNED_CONTEXT((#16702))
GLOBAL_UNIT_ASSIGNED_CONTEXT((#16800,#16802,#16803))
REPRESENTATION_CONTEXT('','3D')
);
#16752=(
GEOMETRIC_REPRESENTATION_CONTEXT(3)
GLOBAL_UNCERTAINTY_ASSIGNED_CONTEXT((#16703))
GLOBAL_UNIT_ASSIGNED_CONTEXT((#16800,#16802,#16803))
REPRESENTATION_CONTEXT('','3D')
);
#16753=(
GEOMETRIC_REPRESENTATION_CONTEXT(3)
GLOBAL_UNCERTAINTY_ASSIGNED_CONTEXT((#16704))
GLOBAL_UNIT_ASSIGNED_CONTEXT((#16800,#16802,#16803))
REPRESENTATION_CONTEXT('','3D')
);
#16754=(
GEOMETRIC_REPRESENTATION_CONTEXT(3)
GLOBAL_UNCERTAINTY_ASSIGNED_CONTEXT((#16705))
GLOBAL_UNIT_ASSIGNED_CONTEXT((#16800,#16802,#16803))
REPRESENTATION_CONTEXT('','3D')
);
#16755=(
GEOMETRIC_REPRESENTATION_CONTEXT(3)
GLOBAL_UNCERTAINTY_ASSIGNED_CONTEXT((#16706))
GLOBAL_UNIT_ASSIGNED_CONTEXT((#16800,#16802,#16803))
REPRESENTATION_CONTEXT('','3D')
);
#16756=(
GEOMETRIC_REPRESENTATION_CONTEXT(3)
GLOBAL_UNCERTAINTY_ASSIGNED_CONTEXT((#16707))
GLOBAL_UNIT_ASSIGNED_CONTEXT((#16800,#16802,#16803))
REPRESENTATION_CONTEXT('','3D')
);
#16757=(
GEOMETRIC_REPRESENTATION_CONTEXT(3)
GLOBAL_UNCERTAINTY_ASSIGNED_CONTEXT((#16708))
GLOBAL_UNIT_ASSIGNED_CONTEXT((#16800,#16802,#16803))
REPRESENTATION_CONTEXT('','3D')
);
#16758=(
GEOMETRIC_REPRESENTATION_CONTEXT(3)
GLOBAL_UNCERTAINTY_ASSIGNED_CONTEXT((#16709))
GLOBAL_UNIT_ASSIGNED_CONTEXT((#16800,#16802,#16803))
REPRESENTATION_CONTEXT('','3D')
);
#16759=(
GEOMETRIC_REPRESENTATION_CONTEXT(3)
GLOBAL_UNCERTAINTY_ASSIGNED_CONTEXT((#16710))
GLOBAL_UNIT_ASSIGNED_CONTEXT((#16800,#16802,#16803))
REPRESENTATION_CONTEXT('','3D')
);
#16760=(
GEOMETRIC_REPRESENTATION_CONTEXT(3)
GLOBAL_UNCERTAINTY_ASSIGNED_CONTEXT((#16711))
GLOBAL_UNIT_ASSIGNED_CONTEXT((#16800,#16802,#16803))
REPRESENTATION_CONTEXT('','3D')
);
#16761=(
GEOMETRIC_REPRESENTATION_CONTEXT(3)
GLOBAL_UNCERTAINTY_ASSIGNED_CONTEXT((#16712))
GLOBAL_UNIT_ASSIGNED_CONTEXT((#16800,#16802,#16803))
REPRESENTATION_CONTEXT('','3D')
);
#16762=(
GEOMETRIC_REPRESENTATION_CONTEXT(3)
GLOBAL_UNCERTAINTY_ASSIGNED_CONTEXT((#16713))
GLOBAL_UNIT_ASSIGNED_CONTEXT((#16800,#16802,#16803))
REPRESENTATION_CONTEXT('','3D')
);
#16763=(
GEOMETRIC_REPRESENTATION_CONTEXT(3)
GLOBAL_UNCERTAINTY_ASSIGNED_CONTEXT((#16714))
GLOBAL_UNIT_ASSIGNED_CONTEXT((#16800,#16802,#16803))
REPRESENTATION_CONTEXT('','3D')
);
#16764=(
GEOMETRIC_REPRESENTATION_CONTEXT(3)
GLOBAL_UNCERTAINTY_ASSIGNED_CONTEXT((#16715))
GLOBAL_UNIT_ASSIGNED_CONTEXT((#16800,#16802,#16803))
REPRESENTATION_CONTEXT('','3D')
);
#16765=(
GEOMETRIC_REPRESENTATION_CONTEXT(3)
GLOBAL_UNCERTAINTY_ASSIGNED_CONTEXT((#16716))
GLOBAL_UNIT_ASSIGNED_CONTEXT((#16800,#16802,#16803))
REPRESENTATION_CONTEXT('','3D')
);
#16766=(
GEOMETRIC_REPRESENTATION_CONTEXT(3)
GLOBAL_UNCERTAINTY_ASSIGNED_CONTEXT((#16717))
GLOBAL_UNIT_ASSIGNED_CONTEXT((#16800,#16802,#16803))
REPRESENTATION_CONTEXT('','3D')
);
#16767=(
GEOMETRIC_REPRESENTATION_CONTEXT(3)
GLOBAL_UNCERTAINTY_ASSIGNED_CONTEXT((#16718))
GLOBAL_UNIT_ASSIGNED_CONTEXT((#16800,#16802,#16803))
REPRESENTATION_CONTEXT('','3D')
);
#16768=(
GEOMETRIC_REPRESENTATION_CONTEXT(3)
GLOBAL_UNCERTAINTY_ASSIGNED_CONTEXT((#16719))
GLOBAL_UNIT_ASSIGNED_CONTEXT((#16800,#16802,#16803))
REPRESENTATION_CONTEXT('','3D')
);
#16769=(
GEOMETRIC_REPRESENTATION_CONTEXT(3)
GLOBAL_UNCERTAINTY_ASSIGNED_CONTEXT((#16720))
GLOBAL_UNIT_ASSIGNED_CONTEXT((#16800,#16802,#16803))
REPRESENTATION_CONTEXT('','3D')
);
#16770=(
GEOMETRIC_REPRESENTATION_CONTEXT(3)
GLOBAL_UNCERTAINTY_ASSIGNED_CONTEXT((#16721))
GLOBAL_UNIT_ASSIGNED_CONTEXT((#16800,#16802,#16803))
REPRESENTATION_CONTEXT('','3D')
);
#16771=(
GEOMETRIC_REPRESENTATION_CONTEXT(3)
GLOBAL_UNCERTAINTY_ASSIGNED_CONTEXT((#16722))
GLOBAL_UNIT_ASSIGNED_CONTEXT((#16800,#16802,#16803))
REPRESENTATION_CONTEXT('','3D')
);
#16772=(
GEOMETRIC_REPRESENTATION_CONTEXT(3)
GLOBAL_UNCERTAINTY_ASSIGNED_CONTEXT((#16723))
GLOBAL_UNIT_ASSIGNED_CONTEXT((#16800,#16802,#16803))
REPRESENTATION_CONTEXT('','3D')
);
#16773=(
GEOMETRIC_REPRESENTATION_CONTEXT(3)
GLOBAL_UNCERTAINTY_ASSIGNED_CONTEXT((#16724))
GLOBAL_UNIT_ASSIGNED_CONTEXT((#16800,#16802,#16803))
REPRESENTATION_CONTEXT('','3D')
);
#16774=(
GEOMETRIC_REPRESENTATION_CONTEXT(3)
GLOBAL_UNCERTAINTY_ASSIGNED_CONTEXT((#16725))
GLOBAL_UNIT_ASSIGNED_CONTEXT((#16800,#16802,#16803))
REPRESENTATION_CONTEXT('','3D')
);
#16775=(
GEOMETRIC_REPRESENTATION_CONTEXT(3)
GLOBAL_UNCERTAINTY_ASSIGNED_CONTEXT((#16726))
GLOBAL_UNIT_ASSIGNED_CONTEXT((#16800,#16802,#16803))
REPRESENTATION_CONTEXT('','3D')
);
#16776=(
GEOMETRIC_REPRESENTATION_CONTEXT(3)
GLOBAL_UNCERTAINTY_ASSIGNED_CONTEXT((#16727))
GLOBAL_UNIT_ASSIGNED_CONTEXT((#16800,#16802,#16803))
REPRESENTATION_CONTEXT('','3D')
);
#16777=(
GEOMETRIC_REPRESENTATION_CONTEXT(3)
GLOBAL_UNCERTAINTY_ASSIGNED_CONTEXT((#16728))
GLOBAL_UNIT_ASSIGNED_CONTEXT((#16800,#16802,#16803))
REPRESENTATION_CONTEXT('','3D')
);
#16778=(
GEOMETRIC_REPRESENTATION_CONTEXT(3)
GLOBAL_UNCERTAINTY_ASSIGNED_CONTEXT((#16729))
GLOBAL_UNIT_ASSIGNED_CONTEXT((#16800,#16802,#16803))
REPRESENTATION_CONTEXT('','3D')
);
#16779=(
GEOMETRIC_REPRESENTATION_CONTEXT(3)
GLOBAL_UNCERTAINTY_ASSIGNED_CONTEXT((#16730))
GLOBAL_UNIT_ASSIGNED_CONTEXT((#16800,#16802,#16803))
REPRESENTATION_CONTEXT('','3D')
);
#16780=(
GEOMETRIC_REPRESENTATION_CONTEXT(3)
GLOBAL_UNCERTAINTY_ASSIGNED_CONTEXT((#16731))
GLOBAL_UNIT_ASSIGNED_CONTEXT((#16800,#16802,#16803))
REPRESENTATION_CONTEXT('','3D')
);
#16781=(
GEOMETRIC_REPRESENTATION_CONTEXT(3)
GLOBAL_UNCERTAINTY_ASSIGNED_CONTEXT((#16732))
GLOBAL_UNIT_ASSIGNED_CONTEXT((#16800,#16802,#16803))
REPRESENTATION_CONTEXT('','3D')
);
#16782=(
GEOMETRIC_REPRESENTATION_CONTEXT(3)
GLOBAL_UNCERTAINTY_ASSIGNED_CONTEXT((#16733))
GLOBAL_UNIT_ASSIGNED_CONTEXT((#16800,#16802,#16803))
REPRESENTATION_CONTEXT('','3D')
);
#16783=(
GEOMETRIC_REPRESENTATION_CONTEXT(3)
GLOBAL_UNCERTAINTY_ASSIGNED_CONTEXT((#16734))
GLOBAL_UNIT_ASSIGNED_CONTEXT((#16800,#16802,#16803))
REPRESENTATION_CONTEXT('','3D')
);
#16784=(
GEOMETRIC_REPRESENTATION_CONTEXT(3)
GLOBAL_UNCERTAINTY_ASSIGNED_CONTEXT((#16735))
GLOBAL_UNIT_ASSIGNED_CONTEXT((#16800,#16802,#16803))
REPRESENTATION_CONTEXT('','3D')
);
#16785=(
GEOMETRIC_REPRESENTATION_CONTEXT(3)
GLOBAL_UNCERTAINTY_ASSIGNED_CONTEXT((#16736))
GLOBAL_UNIT_ASSIGNED_CONTEXT((#16800,#16802,#16803))
REPRESENTATION_CONTEXT('','3D')
);
#16786=(
GEOMETRIC_REPRESENTATION_CONTEXT(3)
GLOBAL_UNCERTAINTY_ASSIGNED_CONTEXT((#16737))
GLOBAL_UNIT_ASSIGNED_CONTEXT((#16800,#16802,#16803))
REPRESENTATION_CONTEXT('','3D')
);
#16787=(
GEOMETRIC_REPRESENTATION_CONTEXT(3)
GLOBAL_UNCERTAINTY_ASSIGNED_CONTEXT((#16738))
GLOBAL_UNIT_ASSIGNED_CONTEXT((#16800,#16802,#16803))
REPRESENTATION_CONTEXT('','3D')
);
#16788=(
GEOMETRIC_REPRESENTATION_CONTEXT(3)
GLOBAL_UNCERTAINTY_ASSIGNED_CONTEXT((#16739))
GLOBAL_UNIT_ASSIGNED_CONTEXT((#16800,#16802,#16803))
REPRESENTATION_CONTEXT('','3D')
);
#16789=(
GEOMETRIC_REPRESENTATION_CONTEXT(3)
GLOBAL_UNCERTAINTY_ASSIGNED_CONTEXT((#16740))
GLOBAL_UNIT_ASSIGNED_CONTEXT((#16800,#16802,#16803))
REPRESENTATION_CONTEXT('','3D')
);
#16790=(
GEOMETRIC_REPRESENTATION_CONTEXT(3)
GLOBAL_UNCERTAINTY_ASSIGNED_CONTEXT((#16741))
GLOBAL_UNIT_ASSIGNED_CONTEXT((#16800,#16802,#16803))
REPRESENTATION_CONTEXT('','3D')
);
#16791=(
GEOMETRIC_REPRESENTATION_CONTEXT(3)
GLOBAL_UNCERTAINTY_ASSIGNED_CONTEXT((#16742))
GLOBAL_UNIT_ASSIGNED_CONTEXT((#16800,#16802,#16803))
REPRESENTATION_CONTEXT('','3D')
);
#16792=(
GEOMETRIC_REPRESENTATION_CONTEXT(3)
GLOBAL_UNCERTAINTY_ASSIGNED_CONTEXT((#16743))
GLOBAL_UNIT_ASSIGNED_CONTEXT((#16800,#16802,#16803))
REPRESENTATION_CONTEXT('','3D')
);
#16793=(
GEOMETRIC_REPRESENTATION_CONTEXT(3)
GLOBAL_UNCERTAINTY_ASSIGNED_CONTEXT((#16744))
GLOBAL_UNIT_ASSIGNED_CONTEXT((#16800,#16802,#16803))
REPRESENTATION_CONTEXT('','3D')
);
#16794=(
GEOMETRIC_REPRESENTATION_CONTEXT(3)
GLOBAL_UNCERTAINTY_ASSIGNED_CONTEXT((#16745))
GLOBAL_UNIT_ASSIGNED_CONTEXT((#16800,#16802,#16803))
REPRESENTATION_CONTEXT('','3D')
);
#16795=(
GEOMETRIC_REPRESENTATION_CONTEXT(3)
GLOBAL_UNCERTAINTY_ASSIGNED_CONTEXT((#16746))
GLOBAL_UNIT_ASSIGNED_CONTEXT((#16800,#16802,#16803))
REPRESENTATION_CONTEXT('','3D')
);
#16796=(
GEOMETRIC_REPRESENTATION_CONTEXT(3)
GLOBAL_UNCERTAINTY_ASSIGNED_CONTEXT((#16747))
GLOBAL_UNIT_ASSIGNED_CONTEXT((#16800,#16802,#16803))
REPRESENTATION_CONTEXT('','3D')
);
#16797=(
GEOMETRIC_REPRESENTATION_CONTEXT(3)
GLOBAL_UNCERTAINTY_ASSIGNED_CONTEXT((#16748))
GLOBAL_UNIT_ASSIGNED_CONTEXT((#16800,#16802,#16803))
REPRESENTATION_CONTEXT('','3D')
);
#16798=(
GEOMETRIC_REPRESENTATION_CONTEXT(3)
GLOBAL_UNCERTAINTY_ASSIGNED_CONTEXT((#16749))
GLOBAL_UNIT_ASSIGNED_CONTEXT((#16800,#16802,#16803))
REPRESENTATION_CONTEXT('','3D')
);
#16799=(
GEOMETRIC_REPRESENTATION_CONTEXT(3)
GLOBAL_UNCERTAINTY_ASSIGNED_CONTEXT((#16750))
GLOBAL_UNIT_ASSIGNED_CONTEXT((#16800,#16802,#16803))
REPRESENTATION_CONTEXT('','3D')
);
#16800=(
LENGTH_UNIT()
NAMED_UNIT(*)
SI_UNIT(.CENTI.,.METRE.)
);
#16801=(
LENGTH_UNIT()
NAMED_UNIT(*)
SI_UNIT($,.METRE.)
);
#16802=(
NAMED_UNIT(*)
PLANE_ANGLE_UNIT()
SI_UNIT($,.RADIAN.)
);
#16803=(
NAMED_UNIT(*)
SI_UNIT($,.STERADIAN.)
SOLID_ANGLE_UNIT()
);
#16804=SHAPE_DEFINITION_REPRESENTATION(#16852,#17013);
#16805=SHAPE_DEFINITION_REPRESENTATION(#16853,#17014);
#16806=SHAPE_DEFINITION_REPRESENTATION(#16854,#17015);
#16807=SHAPE_DEFINITION_REPRESENTATION(#16855,#17016);
#16808=SHAPE_DEFINITION_REPRESENTATION(#16856,#17017);
#16809=SHAPE_DEFINITION_REPRESENTATION(#16857,#17018);
#16810=SHAPE_DEFINITION_REPRESENTATION(#16858,#17019);
#16811=SHAPE_DEFINITION_REPRESENTATION(#16859,#17020);
#16812=SHAPE_DEFINITION_REPRESENTATION(#16860,#17021);
#16813=SHAPE_DEFINITION_REPRESENTATION(#16861,#17022);
#16814=SHAPE_DEFINITION_REPRESENTATION(#16862,#17023);
#16815=SHAPE_DEFINITION_REPRESENTATION(#16863,#17024);
#16816=SHAPE_DEFINITION_REPRESENTATION(#16864,#17025);
#16817=SHAPE_DEFINITION_REPRESENTATION(#16865,#17026);
#16818=SHAPE_DEFINITION_REPRESENTATION(#16866,#17027);
#16819=SHAPE_DEFINITION_REPRESENTATION(#16867,#17028);
#16820=SHAPE_DEFINITION_REPRESENTATION(#16868,#17029);
#16821=SHAPE_DEFINITION_REPRESENTATION(#16869,#17030);
#16822=SHAPE_DEFINITION_REPRESENTATION(#16870,#17031);
#16823=SHAPE_DEFINITION_REPRESENTATION(#16871,#17032);
#16824=SHAPE_DEFINITION_REPRESENTATION(#16872,#17033);
#16825=SHAPE_DEFINITION_REPRESENTATION(#16873,#17034);
#16826=SHAPE_DEFINITION_REPRESENTATION(#16879,#17035);
#16827=SHAPE_DEFINITION_REPRESENTATION(#16880,#17036);
#16828=SHAPE_DEFINITION_REPRESENTATION(#16881,#17037);
#16829=SHAPE_DEFINITION_REPRESENTATION(#16882,#17038);
#16830=SHAPE_DEFINITION_REPRESENTATION(#16883,#17039);
#16831=SHAPE_DEFINITION_REPRESENTATION(#16884,#17040);
#16832=SHAPE_DEFINITION_REPRESENTATION(#16885,#17041);
#16833=SHAPE_DEFINITION_REPRESENTATION(#16886,#17042);
#16834=SHAPE_DEFINITION_REPRESENTATION(#16887,#17043);
#16835=SHAPE_DEFINITION_REPRESENTATION(#16888,#17044);
#16836=SHAPE_DEFINITION_REPRESENTATION(#16889,#17045);
#16837=SHAPE_DEFINITION_REPRESENTATION(#16890,#17046);
#16838=SHAPE_DEFINITION_REPRESENTATION(#16891,#17047);
#16839=SHAPE_DEFINITION_REPRESENTATION(#16892,#17048);
#16840=SHAPE_DEFINITION_REPRESENTATION(#16893,#17049);
#16841=SHAPE_DEFINITION_REPRESENTATION(#16896,#17050);
#16842=SHAPE_DEFINITION_REPRESENTATION(#16897,#17051);
#16843=SHAPE_DEFINITION_REPRESENTATION(#16898,#17052);
#16844=SHAPE_DEFINITION_REPRESENTATION(#16899,#17053);
#16845=SHAPE_DEFINITION_REPRESENTATION(#16900,#17054);
#16846=SHAPE_DEFINITION_REPRESENTATION(#16901,#17055);
#16847=SHAPE_DEFINITION_REPRESENTATION(#16902,#17056);
#16848=SHAPE_DEFINITION_REPRESENTATION(#16903,#17057);
#16849=SHAPE_DEFINITION_REPRESENTATION(#16904,#17058);
#16850=SHAPE_DEFINITION_REPRESENTATION(#16905,#17059);
#16851=SHAPE_DEFINITION_REPRESENTATION(#16948,#17060);
#16852=PRODUCT_DEFINITION_SHAPE('',$,#17062);
#16853=PRODUCT_DEFINITION_SHAPE('',$,#17063);
#16854=PRODUCT_DEFINITION_SHAPE('',$,#17064);
#16855=PRODUCT_DEFINITION_SHAPE('',$,#17065);
#16856=PRODUCT_DEFINITION_SHAPE('',$,#17066);
#16857=PRODUCT_DEFINITION_SHAPE('',$,#17067);
#16858=PRODUCT_DEFINITION_SHAPE('',$,#17068);
#16859=PRODUCT_DEFINITION_SHAPE('',$,#17069);
#16860=PRODUCT_DEFINITION_SHAPE('',$,#17070);
#16861=PRODUCT_DEFINITION_SHAPE('',$,#17071);
#16862=PRODUCT_DEFINITION_SHAPE('',$,#17072);
#16863=PRODUCT_DEFINITION_SHAPE('',$,#17073);
#16864=PRODUCT_DEFINITION_SHAPE('',$,#17074);
#16865=PRODUCT_DEFINITION_SHAPE('',$,#17075);
#16866=PRODUCT_DEFINITION_SHAPE('',$,#17076);
#16867=PRODUCT_DEFINITION_SHAPE('',$,#17077);
#16868=PRODUCT_DEFINITION_SHAPE('',$,#17078);
#16869=PRODUCT_DEFINITION_SHAPE('',$,#17079);
#16870=PRODUCT_DEFINITION_SHAPE('',$,#17080);
#16871=PRODUCT_DEFINITION_SHAPE('',$,#17081);
#16872=PRODUCT_DEFINITION_SHAPE('',$,#17082);
#16873=PRODUCT_DEFINITION_SHAPE('',$,#17083);
#16874=PRODUCT_DEFINITION_SHAPE($,$,#354);
#16875=PRODUCT_DEFINITION_SHAPE($,$,#355);
#16876=PRODUCT_DEFINITION_SHAPE($,$,#356);
#16877=PRODUCT_DEFINITION_SHAPE($,$,#357);
#16878=PRODUCT_DEFINITION_SHAPE($,$,#358);
#16879=PRODUCT_DEFINITION_SHAPE('',$,#17084);
#16880=PRODUCT_DEFINITION_SHAPE('',$,#17085);
#16881=PRODUCT_DEFINITION_SHAPE('',$,#17086);
#16882=PRODUCT_DEFINITION_SHAPE('',$,#17087);
#16883=PRODUCT_DEFINITION_SHAPE('',$,#17088);
#16884=PRODUCT_DEFINITION_SHAPE('',$,#17089);
#16885=PRODUCT_DEFINITION_SHAPE('',$,#17090);
#16886=PRODUCT_DEFINITION_SHAPE('',$,#17091);
#16887=PRODUCT_DEFINITION_SHAPE('',$,#17092);
#16888=PRODUCT_DEFINITION_SHAPE('',$,#17093);
#16889=PRODUCT_DEFINITION_SHAPE('',$,#17094);
#16890=PRODUCT_DEFINITION_SHAPE('',$,#17095);
#16891=PRODUCT_DEFINITION_SHAPE('',$,#17096);
#16892=PRODUCT_DEFINITION_SHAPE('',$,#17097);
#16893=PRODUCT_DEFINITION_SHAPE('',$,#17098);
#16894=PRODUCT_DEFINITION_SHAPE($,$,#359);
#16895=PRODUCT_DEFINITION_SHAPE($,$,#360);
#16896=PRODUCT_DEFINITION_SHAPE('',$,#17099);
#16897=PRODUCT_DEFINITION_SHAPE('',$,#17100);
#16898=PRODUCT_DEFINITION_SHAPE('',$,#17101);
#16899=PRODUCT_DEFINITION_SHAPE('',$,#17102);
#16900=PRODUCT_DEFINITION_SHAPE('',$,#17103);
#16901=PRODUCT_DEFINITION_SHAPE('',$,#17104);
#16902=PRODUCT_DEFINITION_SHAPE('',$,#17105);
#16903=PRODUCT_DEFINITION_SHAPE('',$,#17106);
#16904=PRODUCT_DEFINITION_SHAPE('',$,#17107);
#16905=PRODUCT_DEFINITION_SHAPE('',$,#17108);
#16906=PRODUCT_DEFINITION_SHAPE($,$,#361);
#16907=PRODUCT_DEFINITION_SHAPE($,$,#362);
#16908=PRODUCT_DEFINITION_SHAPE($,$,#363);
#16909=PRODUCT_DEFINITION_SHAPE($,$,#364);
#16910=PRODUCT_DEFINITION_SHAPE($,$,#365);
#16911=PRODUCT_DEFINITION_SHAPE($,$,#366);
#16912=PRODUCT_DEFINITION_SHAPE($,$,#367);
#16913=PRODUCT_DEFINITION_SHAPE($,$,#368);
#16914=PRODUCT_DEFINITION_SHAPE($,$,#369);
#16915=PRODUCT_DEFINITION_SHAPE($,$,#370);
#16916=PRODUCT_DEFINITION_SHAPE($,$,#371);
#16917=PRODUCT_DEFINITION_SHAPE($,$,#372);
#16918=PRODUCT_DEFINITION_SHAPE($,$,#373);
#16919=PRODUCT_DEFINITION_SHAPE($,$,#374);
#16920=PRODUCT_DEFINITION_SHAPE($,$,#375);
#16921=PRODUCT_DEFINITION_SHAPE($,$,#376);
#16922=PRODUCT_DEFINITION_SHAPE($,$,#377);
#16923=PRODUCT_DEFINITION_SHAPE($,$,#378);
#16924=PRODUCT_DEFINITION_SHAPE($,$,#379);
#16925=PRODUCT_DEFINITION_SHAPE($,$,#380);
#16926=PRODUCT_DEFINITION_SHAPE($,$,#381);
#16927=PRODUCT_DEFINITION_SHAPE($,$,#382);
#16928=PRODUCT_DEFINITION_SHAPE($,$,#383);
#16929=PRODUCT_DEFINITION_SHAPE($,$,#384);
#16930=PRODUCT_DEFINITION_SHAPE($,$,#385);
#16931=PRODUCT_DEFINITION_SHAPE($,$,#386);
#16932=PRODUCT_DEFINITION_SHAPE($,$,#387);
#16933=PRODUCT_DEFINITION_SHAPE($,$,#388);
#16934=PRODUCT_DEFINITION_SHAPE($,$,#389);
#16935=PRODUCT_DEFINITION_SHAPE($,$,#390);
#16936=PRODUCT_DEFINITION_SHAPE($,$,#391);
#16937=PRODUCT_DEFINITION_SHAPE($,$,#392);
#16938=PRODUCT_DEFINITION_SHAPE($,$,#393);
#16939=PRODUCT_DEFINITION_SHAPE($,$,#394);
#16940=PRODUCT_DEFINITION_SHAPE($,$,#395);
#16941=PRODUCT_DEFINITION_SHAPE($,$,#396);
#16942=PRODUCT_DEFINITION_SHAPE($,$,#397);
#16943=PRODUCT_DEFINITION_SHAPE($,$,#398);
#16944=PRODUCT_DEFINITION_SHAPE($,$,#399);
#16945=PRODUCT_DEFINITION_SHAPE($,$,#400);
#16946=PRODUCT_DEFINITION_SHAPE($,$,#401);
#16947=PRODUCT_DEFINITION_SHAPE($,$,#402);
#16948=PRODUCT_DEFINITION_SHAPE('',$,#17109);
#16949=PRODUCT_DEFINITION_SHAPE($,$,#403);
#16950=PRODUCT_DEFINITION_SHAPE($,$,#404);
#16951=PRODUCT_DEFINITION_SHAPE($,$,#405);
#16952=PRODUCT_DEFINITION_SHAPE($,$,#406);
#16953=PRODUCT_DEFINITION_SHAPE($,$,#407);
#16954=PRODUCT_DEFINITION_SHAPE($,$,#408);
#16955=PRODUCT_DEFINITION_SHAPE($,$,#409);
#16956=PRODUCT_DEFINITION_SHAPE($,$,#410);
#16957=PRODUCT_DEFINITION_SHAPE($,$,#411);
#16958=PRODUCT_DEFINITION_SHAPE($,$,#412);
#16959=PRODUCT_DEFINITION_SHAPE($,$,#413);
#16960=PRODUCT_DEFINITION_SHAPE($,$,#414);
#16961=PRODUCT_DEFINITION_SHAPE($,$,#415);
#16962=PRODUCT_DEFINITION_SHAPE($,$,#416);
#16963=PRODUCT_DEFINITION_SHAPE($,$,#417);
#16964=PRODUCT_DEFINITION_SHAPE($,$,#418);
#16965=PRODUCT_DEFINITION_SHAPE($,$,#419);
#16966=PRODUCT_DEFINITION_SHAPE($,$,#420);
#16967=PRODUCT_DEFINITION_SHAPE($,$,#421);
#16968=PRODUCT_DEFINITION_SHAPE($,$,#422);
#16969=PRODUCT_DEFINITION_SHAPE($,$,#423);
#16970=PRODUCT_DEFINITION_SHAPE($,$,#424);
#16971=PRODUCT_DEFINITION_SHAPE($,$,#425);
#16972=PRODUCT_DEFINITION_SHAPE($,$,#426);
#16973=PRODUCT_DEFINITION_SHAPE($,$,#427);
#16974=PRODUCT_DEFINITION_SHAPE($,$,#428);
#16975=PRODUCT_DEFINITION_SHAPE($,$,#429);
#16976=PRODUCT_DEFINITION_SHAPE($,$,#430);
#16977=PRODUCT_DEFINITION_SHAPE($,$,#431);
#16978=PRODUCT_DEFINITION_SHAPE($,$,#432);
#16979=PRODUCT_DEFINITION_SHAPE($,$,#433);
#16980=PRODUCT_DEFINITION_SHAPE($,$,#434);
#16981=PRODUCT_DEFINITION_SHAPE($,$,#435);
#16982=PRODUCT_DEFINITION_SHAPE($,$,#436);
#16983=PRODUCT_DEFINITION_SHAPE($,$,#437);
#16984=PRODUCT_DEFINITION_SHAPE($,$,#438);
#16985=PRODUCT_DEFINITION_SHAPE($,$,#439);
#16986=PRODUCT_DEFINITION_SHAPE($,$,#440);
#16987=PRODUCT_DEFINITION_SHAPE($,$,#441);
#16988=PRODUCT_DEFINITION_SHAPE($,$,#442);
#16989=PRODUCT_DEFINITION_SHAPE($,$,#443);
#16990=PRODUCT_DEFINITION_SHAPE($,$,#444);
#16991=PRODUCT_DEFINITION_SHAPE($,$,#445);
#16992=PRODUCT_DEFINITION_SHAPE($,$,#446);
#16993=PRODUCT_DEFINITION_SHAPE($,$,#447);
#16994=PRODUCT_DEFINITION_SHAPE($,$,#448);
#16995=PRODUCT_DEFINITION_SHAPE($,$,#449);
#16996=PRODUCT_DEFINITION_SHAPE($,$,#450);
#16997=PRODUCT_DEFINITION_SHAPE($,$,#451);
#16998=PRODUCT_DEFINITION_SHAPE($,$,#452);
#16999=PRODUCT_DEFINITION_SHAPE($,$,#453);
#17000=PRODUCT_DEFINITION_SHAPE($,$,#454);
#17001=PRODUCT_DEFINITION_SHAPE($,$,#455);
#17002=PRODUCT_DEFINITION_SHAPE($,$,#456);
#17003=PRODUCT_DEFINITION_SHAPE($,$,#457);
#17004=PRODUCT_DEFINITION_SHAPE($,$,#458);
#17005=PRODUCT_DEFINITION_SHAPE($,$,#459);
#17006=PRODUCT_DEFINITION_SHAPE($,$,#460);
#17007=PRODUCT_DEFINITION_SHAPE($,$,#461);
#17008=PRODUCT_DEFINITION_SHAPE($,$,#462);
#17009=PRODUCT_DEFINITION_SHAPE($,$,#463);
#17010=PRODUCT_DEFINITION_SHAPE($,$,#464);
#17011=PRODUCT_DEFINITION_SHAPE($,$,#465);
#17012=PRODUCT_DEFINITION_SHAPE($,$,#466);
#17013=SHAPE_REPRESENTATION('',(#9577,#10748,#10749,#10750,#10751),#16751);
#17014=SHAPE_REPRESENTATION('',(#9578,#10688,#10689,#10690,#10691,#10692,
#10693,#10694,#10695,#10696,#10697,#10698,#10699,#10700,#10701,#10702,#10703,
#10704,#10705,#10706,#10707,#10708,#10709,#10710,#10711,#10712,#10713,#10714,
#10715,#10716,#10717,#10718,#10719,#10720,#10721,#10722,#10723,#10724,#10725,
#10726,#10727,#10728,#10729,#10730,#10731,#10732,#10733,#10734,#10735,#10736),
#16752);
#17015=SHAPE_REPRESENTATION('',(#9579),#16753);
#17016=SHAPE_REPRESENTATION('',(#9622),#16754);
#17017=SHAPE_REPRESENTATION('',(#9629),#16755);
#17018=SHAPE_REPRESENTATION('',(#9636),#16756);
#17019=SHAPE_REPRESENTATION('',(#9672),#16757);
#17020=SHAPE_REPRESENTATION('',(#9708),#16758);
#17021=SHAPE_REPRESENTATION('',(#9744),#16759);
#17022=SHAPE_REPRESENTATION('',(#9780),#16760);
#17023=SHAPE_REPRESENTATION('',(#9812),#16761);
#17024=SHAPE_REPRESENTATION('',(#9837),#16762);
#17025=SHAPE_REPRESENTATION('',(#9862),#16763);
#17026=SHAPE_REPRESENTATION('',(#9894),#16764);
#17027=SHAPE_REPRESENTATION('',(#9919),#16765);
#17028=SHAPE_REPRESENTATION('',(#9944),#16766);
#17029=SHAPE_REPRESENTATION('',(#9954,#10077,#10078,#10079,#10080,#10081),
#16767);
#17030=SHAPE_REPRESENTATION('',(#9955),#16768);
#17031=SHAPE_REPRESENTATION('',(#9975),#16769);
#17032=SHAPE_REPRESENTATION('',(#9995),#16770);
#17033=SHAPE_REPRESENTATION('',(#10010),#16771);
#17034=SHAPE_REPRESENTATION('',(#10060),#16772);
#17035=SHAPE_REPRESENTATION('',(#10082,#10629,#10630,#10631,#10632,#10633,
#10634,#10635,#10636,#10637,#10638,#10639,#10640,#10641,#10642,#10643,#10644,
#10645,#10646,#10647,#10648,#10649),#16773);
#17036=SHAPE_REPRESENTATION('',(#10083),#16774);
#17037=SHAPE_REPRESENTATION('',(#10135),#16775);
#17038=SHAPE_REPRESENTATION('',(#10163),#16776);
#17039=SHAPE_REPRESENTATION('',(#10191),#16777);
#17040=SHAPE_REPRESENTATION('',(#10220),#16778);
#17041=SHAPE_REPRESENTATION('',(#10255,#10650,#10651,#10652,#10653,#10654,
#10655,#10656,#10657,#10658,#10659,#10660,#10661,#10662,#10663,#10664,#10665,
#10666,#10667,#10668,#10669,#10670),#16779);
#17042=SHAPE_REPRESENTATION('',(#10256),#16780);
#17043=SHAPE_REPRESENTATION('',(#10308),#16781);
#17044=SHAPE_REPRESENTATION('',(#10336),#16782);
#17045=SHAPE_REPRESENTATION('',(#10364),#16783);
#17046=SHAPE_REPRESENTATION('',(#10393),#16784);
#17047=SHAPE_REPRESENTATION('',(#10428,#10478,#10479),#16785);
#17048=SHAPE_REPRESENTATION('',(#10429),#16786);
#17049=SHAPE_REPRESENTATION('',(#10461),#16787);
#17050=SHAPE_REPRESENTATION('',(#10480),#16788);
#17051=SHAPE_REPRESENTATION('',(#10504,#10737,#10738,#10739,#10740,#10741,
#10742,#10743,#10744,#10745,#10746,#10747),#16789);
#17052=SHAPE_REPRESENTATION('',(#10505),#16790);
#17053=SHAPE_REPRESENTATION('',(#10535),#16791);
#17054=SHAPE_REPRESENTATION('',(#10544),#16792);
#17055=SHAPE_REPRESENTATION('',(#10553),#16793);
#17056=SHAPE_REPRESENTATION('',(#10571),#16794);
#17057=SHAPE_REPRESENTATION('',(#10580),#16795);
#17058=SHAPE_REPRESENTATION('',(#10589),#16796);
#17059=SHAPE_REPRESENTATION('',(#10603),#16797);
#17060=SHAPE_REPRESENTATION('',(#10671),#16798);
#17061=PRODUCT_DEFINITION_CONTEXT('part definition',#17207,'design');
#17062=PRODUCT_DEFINITION('PAT-093','PAT-093',#17110,
#17061);
#17063=PRODUCT_DEFINITION('Base, shafts and bearings',
'Base, shafts and bearings',#17111,#17061);
#17064=PRODUCT_DEFINITION('Base','Base',#17112,#17061);
#17065=PRODUCT_DEFINITION('Foot strip','Foot strip',#17113,#17061);
#17066=PRODUCT_DEFINITION('Foot strip (1)','Foot strip (1)',#17114,#17061);
#17067=PRODUCT_DEFINITION('Guide shaft support','Guide shaft support',#17115,
#17061);
#17068=PRODUCT_DEFINITION('Guide shaft support (1)',
'Guide shaft support (1)',#17116,#17061);
#17069=PRODUCT_DEFINITION('Guide shaft support (2)',
'Guide shaft support (2)',#17117,#17061);
#17070=PRODUCT_DEFINITION('Guide shaft support (3)',
'Guide shaft support (3)',#17118,#17061);
#17071=PRODUCT_DEFINITION('Screw bearing post','Screw bearing post',#17119,
#17061);
#17072=PRODUCT_DEFINITION('Bearing cap','Bearing cap',#17120,#17061);
#17073=PRODUCT_DEFINITION('Bearing cap (1)','Bearing cap (1)',#17121,#17061);
#17074=PRODUCT_DEFINITION('Screw bearing post (1)',
'Screw bearing post (1)',#17122,#17061);
#17075=PRODUCT_DEFINITION('Bearing cap (2)','Bearing cap (2)',#17123,#17061);
#17076=PRODUCT_DEFINITION('Bearing cap (3)','Bearing cap (3)',#17124,#17061);
#17077=PRODUCT_DEFINITION(
'Precision Shaft - 12 mm Diameter, 300 mm Long',
'Precision Shaft - 12 mm Diameter, 300 mm Long',#17125,#17061);
#17078=PRODUCT_DEFINITION('Sealed Ball Bearing - 12 x 32 x 10 mm',
'Sealed Ball Bearing - 12 x 32 x 10 mm',#17126,#17061);
#17079=PRODUCT_DEFINITION('Inner ring','Inner ring',#17127,#17061);
#17080=PRODUCT_DEFINITION('Outer ring','Outer ring',#17128,#17061);
#17081=PRODUCT_DEFINITION('Balls','Balls',#17129,#17061);
#17082=PRODUCT_DEFINITION('Cage','Cage',#17130,#17061);
#17083=PRODUCT_DEFINITION('Seals 2RS','Seals 2RS',#17131,#17061);
#17084=PRODUCT_DEFINITION('Left moving jaw','Left moving jaw',#17132,#17061);
#17085=PRODUCT_DEFINITION('Left jaw body','Left jaw body',#17133,#17061);
#17086=PRODUCT_DEFINITION('Jaw guide cap','Jaw guide cap',#17134,#17061);
#17087=PRODUCT_DEFINITION('Jaw guide cap (1)','Jaw guide cap (1)',#17135,
#17061);
#17088=PRODUCT_DEFINITION('Left screw nut','Left screw nut',#17136,#17061);
#17089=PRODUCT_DEFINITION('Left jaw plate','Left jaw plate',#17137,#17061);
#17090=PRODUCT_DEFINITION('Right moving jaw','Right moving jaw',#17138,
#17061);
#17091=PRODUCT_DEFINITION('Right jaw body','Right jaw body',#17139,#17061);
#17092=PRODUCT_DEFINITION('Jaw guide cap (2)','Jaw guide cap (2)',#17140,
#17061);
#17093=PRODUCT_DEFINITION('Jaw guide cap (3)','Jaw guide cap (3)',#17141,
#17061);
#17094=PRODUCT_DEFINITION('Right screw nut','Right screw nut',#17142,#17061);
#17095=PRODUCT_DEFINITION('Right jaw plate','Right jaw plate',#17143,#17061);
#17096=PRODUCT_DEFINITION('Linear Ball Bushing - 12 x 21 x 30 mm',
'Linear Ball Bushing - 12 x 21 x 30 mm',#17144,#17061);
#17097=PRODUCT_DEFINITION('Steel sleeve','Steel sleeve',#17145,#17061);
#17098=PRODUCT_DEFINITION('Ball retainer (plastic)',
'Ball retainer (plastic)',#17146,#17061);
#17099=PRODUCT_DEFINITION('M4x10 Cap Screw','M4x10 Cap Screw',#17147,#17061);
#17100=PRODUCT_DEFINITION('Opposed screw and handwheel',
'Opposed screw and handwheel',#17148,#17061);
#17101=PRODUCT_DEFINITION('Opposed M12 x 3 screw envelope',
'Opposed M12 x 3 screw envelope',#17149,#17061);
#17102=PRODUCT_DEFINITION('Outer bearing sleeve','Outer bearing sleeve',
#17150,#17061);
#17103=PRODUCT_DEFINITION('Outer bearing sleeve (1)',
'Outer bearing sleeve (1)',#17151,#17061);
#17104=PRODUCT_DEFINITION('Handwheel','Handwheel',#17152,#17061);
#17105=PRODUCT_DEFINITION('Shaft keeper','Shaft keeper',#17153,#17061);
#17106=PRODUCT_DEFINITION('Shaft keeper (1)','Shaft keeper (1)',#17154,#17061);
#17107=PRODUCT_DEFINITION('Right end collar','Right end collar',#17155,
#17061);
#17108=PRODUCT_DEFINITION('Cap Screw - M4x16','Cap Screw - M4x16',#17156,
#17061);
#17109=PRODUCT_DEFINITION('Socket Set Screw - M4x6',
'Socket Set Screw - M4x6',#17157,#17061);
#17110=PRODUCT_DEFINITION_FORMATION('',$,#17209);
#17111=PRODUCT_DEFINITION_FORMATION('',$,#17210);
#17112=PRODUCT_DEFINITION_FORMATION('',$,#17211);
#17113=PRODUCT_DEFINITION_FORMATION('',$,#17212);
#17114=PRODUCT_DEFINITION_FORMATION('',$,#17213);
#17115=PRODUCT_DEFINITION_FORMATION('',$,#17214);
#17116=PRODUCT_DEFINITION_FORMATION('',$,#17215);
#17117=PRODUCT_DEFINITION_FORMATION('',$,#17216);
#17118=PRODUCT_DEFINITION_FORMATION('',$,#17217);
#17119=PRODUCT_DEFINITION_FORMATION('',$,#17218);
#17120=PRODUCT_DEFINITION_FORMATION('',$,#17219);
#17121=PRODUCT_DEFINITION_FORMATION('',$,#17220);
#17122=PRODUCT_DEFINITION_FORMATION('',$,#17221);
#17123=PRODUCT_DEFINITION_FORMATION('',$,#17222);
#17124=PRODUCT_DEFINITION_FORMATION('',$,#17223);
#17125=PRODUCT_DEFINITION_FORMATION('',$,#17224);
#17126=PRODUCT_DEFINITION_FORMATION('',$,#17225);
#17127=PRODUCT_DEFINITION_FORMATION('',$,#17226);
#17128=PRODUCT_DEFINITION_FORMATION('',$,#17227);
#17129=PRODUCT_DEFINITION_FORMATION('',$,#17228);
#17130=PRODUCT_DEFINITION_FORMATION('',$,#17229);
#17131=PRODUCT_DEFINITION_FORMATION('',$,#17230);
#17132=PRODUCT_DEFINITION_FORMATION('',$,#17231);
#17133=PRODUCT_DEFINITION_FORMATION('',$,#17232);
#17134=PRODUCT_DEFINITION_FORMATION('',$,#17233);
#17135=PRODUCT_DEFINITION_FORMATION('',$,#17234);
#17136=PRODUCT_DEFINITION_FORMATION('',$,#17235);
#17137=PRODUCT_DEFINITION_FORMATION('',$,#17236);
#17138=PRODUCT_DEFINITION_FORMATION('',$,#17237);
#17139=PRODUCT_DEFINITION_FORMATION('',$,#17238);
#17140=PRODUCT_DEFINITION_FORMATION('',$,#17239);
#17141=PRODUCT_DEFINITION_FORMATION('',$,#17240);
#17142=PRODUCT_DEFINITION_FORMATION('',$,#17241);
#17143=PRODUCT_DEFINITION_FORMATION('',$,#17242);
#17144=PRODUCT_DEFINITION_FORMATION('',$,#17243);
#17145=PRODUCT_DEFINITION_FORMATION('',$,#17244);
#17146=PRODUCT_DEFINITION_FORMATION('',$,#17245);
#17147=PRODUCT_DEFINITION_FORMATION('',$,#17246);
#17148=PRODUCT_DEFINITION_FORMATION('',$,#17247);
#17149=PRODUCT_DEFINITION_FORMATION('',$,#17248);
#17150=PRODUCT_DEFINITION_FORMATION('',$,#17249);
#17151=PRODUCT_DEFINITION_FORMATION('',$,#17250);
#17152=PRODUCT_DEFINITION_FORMATION('',$,#17251);
#17153=PRODUCT_DEFINITION_FORMATION('',$,#17252);
#17154=PRODUCT_DEFINITION_FORMATION('',$,#17253);
#17155=PRODUCT_DEFINITION_FORMATION('',$,#17254);
#17156=PRODUCT_DEFINITION_FORMATION('',$,#17255);
#17157=PRODUCT_DEFINITION_FORMATION('',$,#17256);
#17158=PRODUCT_RELATED_PRODUCT_CATEGORY('PAT-093','PAT-093',(#17209));
#17159=PRODUCT_RELATED_PRODUCT_CATEGORY('Base, shafts and bearings',
'Base, shafts and bearings',(#17210));
#17160=PRODUCT_RELATED_PRODUCT_CATEGORY('Base','Base',(#17211));
#17161=PRODUCT_RELATED_PRODUCT_CATEGORY('Foot strip','Foot strip',(#17212));
#17162=PRODUCT_RELATED_PRODUCT_CATEGORY('Foot strip (1)',
'Foot strip (1)',(#17213));
#17163=PRODUCT_RELATED_PRODUCT_CATEGORY('Guide shaft support',
'Guide shaft support',(#17214));
#17164=PRODUCT_RELATED_PRODUCT_CATEGORY('Guide shaft support (1)',
'Guide shaft support (1)',(#17215));
#17165=PRODUCT_RELATED_PRODUCT_CATEGORY('Guide shaft support (2)',
'Guide shaft support (2)',(#17216));
#17166=PRODUCT_RELATED_PRODUCT_CATEGORY('Guide shaft support (3)',
'Guide shaft support (3)',(#17217));
#17167=PRODUCT_RELATED_PRODUCT_CATEGORY('Screw bearing post',
'Screw bearing post',(#17218));
#17168=PRODUCT_RELATED_PRODUCT_CATEGORY('Bearing cap','Bearing cap',(#17219));
#17169=PRODUCT_RELATED_PRODUCT_CATEGORY('Bearing cap (1)',
'Bearing cap (1)',(#17220));
#17170=PRODUCT_RELATED_PRODUCT_CATEGORY('Screw bearing post (1)',
'Screw bearing post (1)',(#17221));
#17171=PRODUCT_RELATED_PRODUCT_CATEGORY('Bearing cap (2)',
'Bearing cap (2)',(#17222));
#17172=PRODUCT_RELATED_PRODUCT_CATEGORY('Bearing cap (3)',
'Bearing cap (3)',(#17223));
#17173=PRODUCT_RELATED_PRODUCT_CATEGORY(
'Precision Shaft - 12 mm Diameter, 300 mm Long',
'Precision Shaft - 12 mm Diameter, 300 mm Long',(#17224));
#17174=PRODUCT_RELATED_PRODUCT_CATEGORY(
'Sealed Ball Bearing - 12 x 32 x 10 mm',
'Sealed Ball Bearing - 12 x 32 x 10 mm',(#17225));
#17175=PRODUCT_RELATED_PRODUCT_CATEGORY('Inner ring','Inner ring',(#17226));
#17176=PRODUCT_RELATED_PRODUCT_CATEGORY('Outer ring','Outer ring',(#17227));
#17177=PRODUCT_RELATED_PRODUCT_CATEGORY('Balls','Balls',(#17228));
#17178=PRODUCT_RELATED_PRODUCT_CATEGORY('Cage','Cage',(#17229));
#17179=PRODUCT_RELATED_PRODUCT_CATEGORY('Seals 2RS','Seals 2RS',(#17230));
#17180=PRODUCT_RELATED_PRODUCT_CATEGORY('Left moving jaw',
'Left moving jaw',(#17231));
#17181=PRODUCT_RELATED_PRODUCT_CATEGORY('Left jaw body','Left jaw body',
(#17232));
#17182=PRODUCT_RELATED_PRODUCT_CATEGORY('Jaw guide cap','Jaw guide cap',
(#17233));
#17183=PRODUCT_RELATED_PRODUCT_CATEGORY('Jaw guide cap (1)',
'Jaw guide cap (1)',(#17234));
#17184=PRODUCT_RELATED_PRODUCT_CATEGORY('Left screw nut',
'Left screw nut',(#17235));
#17185=PRODUCT_RELATED_PRODUCT_CATEGORY('Left jaw plate',
'Left jaw plate',(#17236));
#17186=PRODUCT_RELATED_PRODUCT_CATEGORY('Right moving jaw',
'Right moving jaw',(#17237));
#17187=PRODUCT_RELATED_PRODUCT_CATEGORY('Right jaw body',
'Right jaw body',(#17238));
#17188=PRODUCT_RELATED_PRODUCT_CATEGORY('Jaw guide cap (2)',
'Jaw guide cap (2)',(#17239));
#17189=PRODUCT_RELATED_PRODUCT_CATEGORY('Jaw guide cap (3)',
'Jaw guide cap (3)',(#17240));
#17190=PRODUCT_RELATED_PRODUCT_CATEGORY('Right screw nut',
'Right screw nut',(#17241));
#17191=PRODUCT_RELATED_PRODUCT_CATEGORY('Right jaw plate',
'Right jaw plate',(#17242));
#17192=PRODUCT_RELATED_PRODUCT_CATEGORY(
'Linear Ball Bushing - 12 x 21 x 30 mm',
'Linear Ball Bushing - 12 x 21 x 30 mm',(#17243));
#17193=PRODUCT_RELATED_PRODUCT_CATEGORY('Steel sleeve','Steel sleeve',(#17244));
#17194=PRODUCT_RELATED_PRODUCT_CATEGORY('Ball retainer (plastic)',
'Ball retainer (plastic)',(#17245));
#17195=PRODUCT_RELATED_PRODUCT_CATEGORY('M4x10 Cap Screw',
'M4x10 Cap Screw',(#17246));
#17196=PRODUCT_RELATED_PRODUCT_CATEGORY('Opposed screw and handwheel',
'Opposed screw and handwheel',(#17247));
#17197=PRODUCT_RELATED_PRODUCT_CATEGORY(
'Opposed M12 x 3 screw envelope','Opposed M12 x 3 screw envelope',(#17248));
#17198=PRODUCT_RELATED_PRODUCT_CATEGORY('Outer bearing sleeve',
'Outer bearing sleeve',(#17249));
#17199=PRODUCT_RELATED_PRODUCT_CATEGORY('Outer bearing sleeve (1)',
'Outer bearing sleeve (1)',(#17250));
#17200=PRODUCT_RELATED_PRODUCT_CATEGORY('Handwheel','Handwheel',(#17251));
#17201=PRODUCT_RELATED_PRODUCT_CATEGORY('Shaft keeper','Shaft keeper',(#17252));
#17202=PRODUCT_RELATED_PRODUCT_CATEGORY('Shaft keeper (1)',
'Shaft keeper (1)',(#17253));
#17203=PRODUCT_RELATED_PRODUCT_CATEGORY('Right end collar',
'Right end collar',(#17254));
#17204=PRODUCT_RELATED_PRODUCT_CATEGORY('Cap Screw - M4x16',
'Cap Screw - M4x16',(#17255));
#17205=PRODUCT_RELATED_PRODUCT_CATEGORY('Socket Set Screw - M4x6',
'Socket Set Screw - M4x6',(#17256));
#17206=APPLICATION_PROTOCOL_DEFINITION('international standard',
'automotive_design',2009,#17207);
#17207=APPLICATION_CONTEXT(
'Core Data for Automotive Mechanical Design Process');
#17208=PRODUCT_CONTEXT('part definition',#17207,'mechanical');
#17209=PRODUCT('PAT-093','PAT-093',
'PAT-093',(#17208));
#17210=PRODUCT('Base, shafts and bearings','Base, shafts and bearings',
'Base, shafts and bearings',(#17208));
#17211=PRODUCT('Base','Base','Base',(#17208));
#17212=PRODUCT('Foot strip','Foot strip','Foot strip',(#17208));
#17213=PRODUCT('Foot strip (1)','Foot strip (1)','Foot strip (1)',(#17208));
#17214=PRODUCT('Guide shaft support','Guide shaft support',
'Guide shaft support',(#17208));
#17215=PRODUCT('Guide shaft support (1)','Guide shaft support (1)',
'Guide shaft support (1)',(#17208));
#17216=PRODUCT('Guide shaft support (2)','Guide shaft support (2)',
'Guide shaft support (2)',(#17208));
#17217=PRODUCT('Guide shaft support (3)','Guide shaft support (3)',
'Guide shaft support (3)',(#17208));
#17218=PRODUCT('Screw bearing post','Screw bearing post',
'Screw bearing post',(#17208));
#17219=PRODUCT('Bearing cap','Bearing cap','Bearing cap',(#17208));
#17220=PRODUCT('Bearing cap (1)','Bearing cap (1)','Bearing cap (1)',(#17208));
#17221=PRODUCT('Screw bearing post (1)','Screw bearing post (1)',
'Screw bearing post (1)',(#17208));
#17222=PRODUCT('Bearing cap (2)','Bearing cap (2)','Bearing cap (2)',(#17208));
#17223=PRODUCT('Bearing cap (3)','Bearing cap (3)','Bearing cap (3)',(#17208));
#17224=PRODUCT('Precision Shaft - 12 mm Diameter, 300 mm Long',
'Precision Shaft - 12 mm Diameter, 300 mm Long',
'Precision Shaft - 12 mm Diameter, 300 mm Long',(#17208));
#17225=PRODUCT('Sealed Ball Bearing - 12 x 32 x 10 mm',
'Sealed Ball Bearing - 12 x 32 x 10 mm',
'Sealed Ball Bearing - 12 x 32 x 10 mm',(#17208));
#17226=PRODUCT('Inner ring','Inner ring','Inner ring',(#17208));
#17227=PRODUCT('Outer ring','Outer ring','Outer ring',(#17208));
#17228=PRODUCT('Balls','Balls','Balls',(#17208));
#17229=PRODUCT('Cage','Cage','Cage',(#17208));
#17230=PRODUCT('Seals 2RS','Seals 2RS','Seals 2RS',(#17208));
#17231=PRODUCT('Left moving jaw','Left moving jaw','Left moving jaw',(#17208));
#17232=PRODUCT('Left jaw body','Left jaw body','Left jaw body',(#17208));
#17233=PRODUCT('Jaw guide cap','Jaw guide cap','Jaw guide cap',(#17208));
#17234=PRODUCT('Jaw guide cap (1)','Jaw guide cap (1)','Jaw guide cap (1)',(#17208));
#17235=PRODUCT('Left screw nut','Left screw nut','Left screw nut',(#17208));
#17236=PRODUCT('Left jaw plate','Left jaw plate','Left jaw plate',(#17208));
#17237=PRODUCT('Right moving jaw','Right moving jaw','Right moving jaw',
(#17208));
#17238=PRODUCT('Right jaw body','Right jaw body','Right jaw body',(#17208));
#17239=PRODUCT('Jaw guide cap (2)','Jaw guide cap (2)','Jaw guide cap (2)',(#17208));
#17240=PRODUCT('Jaw guide cap (3)','Jaw guide cap (3)','Jaw guide cap (3)',(#17208));
#17241=PRODUCT('Right screw nut','Right screw nut','Right screw nut',(#17208));
#17242=PRODUCT('Right jaw plate','Right jaw plate','Right jaw plate',(#17208));
#17243=PRODUCT('Linear Ball Bushing - 12 x 21 x 30 mm',
'Linear Ball Bushing - 12 x 21 x 30 mm',
'Linear Ball Bushing - 12 x 21 x 30 mm',(#17208));
#17244=PRODUCT('Steel sleeve','Steel sleeve','Steel sleeve',(#17208));
#17245=PRODUCT('Ball retainer (plastic)','Ball retainer (plastic)',
'Ball retainer (plastic)',(#17208));
#17246=PRODUCT('M4x10 Cap Screw','M4x10 Cap Screw','M4x10 Cap Screw',(#17208));
#17247=PRODUCT('Opposed screw and handwheel',
'Opposed screw and handwheel','Opposed screw and handwheel',(#17208));
#17248=PRODUCT('Opposed M12 x 3 screw envelope',
'Opposed M12 x 3 screw envelope','Opposed M12 x 3 screw envelope',(#17208));
#17249=PRODUCT('Outer bearing sleeve','Outer bearing sleeve',
'Outer bearing sleeve',(#17208));
#17250=PRODUCT('Outer bearing sleeve (1)','Outer bearing sleeve (1)',
'Outer bearing sleeve (1)',(#17208));
#17251=PRODUCT('Handwheel','Handwheel','Handwheel',(#17208));
#17252=PRODUCT('Shaft keeper','Shaft keeper','Shaft keeper',(#17208));
#17253=PRODUCT('Shaft keeper (1)','Shaft keeper (1)','Shaft keeper (1)',(#17208));
#17254=PRODUCT('Right end collar','Right end collar','Right end collar',
(#17208));
#17255=PRODUCT('Cap Screw - M4x16','Cap Screw - M4x16',
'Cap Screw - M4x16',(#17208));
#17256=PRODUCT('Socket Set Screw - M4x6','Socket Set Screw - M4x6',
'Socket Set Screw - M4x6',(#17208));
#17257=PRESENTATION_STYLE_ASSIGNMENT((#17263));
#17258=PRESENTATION_STYLE_ASSIGNMENT((#17264));
#17259=PRESENTATION_STYLE_ASSIGNMENT((#17265));
#17260=PRESENTATION_STYLE_ASSIGNMENT((#17266));
#17261=PRESENTATION_STYLE_ASSIGNMENT((#17267));
#17262=PRESENTATION_STYLE_ASSIGNMENT((#17268));
#17263=SURFACE_STYLE_USAGE(.BOTH.,#17269);
#17264=SURFACE_STYLE_USAGE(.BOTH.,#17270);
#17265=SURFACE_STYLE_USAGE(.BOTH.,#17271);
#17266=SURFACE_STYLE_USAGE(.BOTH.,#17272);
#17267=SURFACE_STYLE_USAGE(.BOTH.,#17273);
#17268=SURFACE_STYLE_USAGE(.BOTH.,#17274);
#17269=SURFACE_SIDE_STYLE('',(#17275));
#17270=SURFACE_SIDE_STYLE('',(#17276));
#17271=SURFACE_SIDE_STYLE('',(#17277));
#17272=SURFACE_SIDE_STYLE('',(#17278));
#17273=SURFACE_SIDE_STYLE('',(#17279));
#17274=SURFACE_SIDE_STYLE('',(#17280));
#17275=SURFACE_STYLE_FILL_AREA(#17281);
#17276=SURFACE_STYLE_FILL_AREA(#17282);
#17277=SURFACE_STYLE_FILL_AREA(#17283);
#17278=SURFACE_STYLE_FILL_AREA(#17284);
#17279=SURFACE_STYLE_FILL_AREA(#17285);
#17280=SURFACE_STYLE_FILL_AREA(#17286);
#17281=FILL_AREA_STYLE('Steel - Satin',(#17287));
#17282=FILL_AREA_STYLE('CAD Library Painted - Deep blue',(#17288));
#17283=FILL_AREA_STYLE('CAD Library Painted - Steel gray',(#17289));
#17284=FILL_AREA_STYLE('CAD Library Painted - Graphite',(#17290));
#17285=FILL_AREA_STYLE('CAD Library Painted - Engineering blue',(#17291));
#17286=FILL_AREA_STYLE('CAD Library Painted - Light blue',(#17292));
#17287=FILL_AREA_STYLE_COLOUR('Steel - Satin',#17293);
#17288=FILL_AREA_STYLE_COLOUR('CAD Library Painted - Deep blue',#17294);
#17289=FILL_AREA_STYLE_COLOUR('CAD Library Painted - Steel gray',#17295);
#17290=FILL_AREA_STYLE_COLOUR('CAD Library Painted - Graphite',#17296);
#17291=FILL_AREA_STYLE_COLOUR('CAD Library Painted - Engineering blue',
#17297);
#17292=FILL_AREA_STYLE_COLOUR('CAD Library Painted - Light blue',#17298);
#17293=COLOUR_RGB('Steel - Satin',0.627450980392157,0.627450980392157,0.627450980392157);
#17294=COLOUR_RGB('CAD Library Painted - Deep blue',0.0784313725490196,
0.203921568627451,0.349019607843137);
#17295=COLOUR_RGB('CAD Library Painted - Steel gray',0.592156862745098,
0.631372549019608,0.67843137254902);
#17296=COLOUR_RGB('CAD Library Painted - Graphite',0.168627450980392,0.192156862745098,
0.231372549019608);
#17297=COLOUR_RGB('CAD Library Painted - Engineering blue',0.12156862745098,
0.356862745098039,0.6);
#17298=COLOUR_RGB('CAD Library Painted - Light blue',0.286274509803922,
0.552941176470588,0.780392156862745);
#17299=COLOUR_RGB('Dark Blue',0.08,0.2,0.34);
#17300=FILL_AREA_STYLE_COLOUR('',#17299);
#17301=FILL_AREA_STYLE('',(#17300));
#17302=SURFACE_STYLE_FILL_AREA(#17301);
#17303=SURFACE_SIDE_STYLE('',(#17302));
#17304=SURFACE_STYLE_USAGE(.BOTH.,#17303);
#17305=PRESENTATION_STYLE_ASSIGNMENT((#17304));
#17306=COLOUR_RGB('Light Blue',0.38,0.62,0.78);
#17307=FILL_AREA_STYLE_COLOUR('',#17306);
#17308=FILL_AREA_STYLE('',(#17307));
#17309=SURFACE_STYLE_FILL_AREA(#17308);
#17310=SURFACE_SIDE_STYLE('',(#17309));
#17311=SURFACE_STYLE_USAGE(.BOTH.,#17310);
#17312=PRESENTATION_STYLE_ASSIGNMENT((#17311));
#17313=COLOUR_RGB('Sky Blue',0.24,0.69,0.87);
#17314=FILL_AREA_STYLE_COLOUR('',#17313);
#17315=FILL_AREA_STYLE('',(#17314));
#17316=SURFACE_STYLE_FILL_AREA(#17315);
#17317=SURFACE_SIDE_STYLE('',(#17316));
#17318=SURFACE_STYLE_USAGE(.BOTH.,#17317);
#17319=PRESENTATION_STYLE_ASSIGNMENT((#17318));
#17320=COLOUR_RGB('Grey',0.48,0.52,0.57);
#17321=FILL_AREA_STYLE_COLOUR('',#17320);
#17322=FILL_AREA_STYLE('',(#17321));
#17323=SURFACE_STYLE_FILL_AREA(#17322);
#17324=SURFACE_SIDE_STYLE('',(#17323));
#17325=SURFACE_STYLE_USAGE(.BOTH.,#17324);
#17326=PRESENTATION_STYLE_ASSIGNMENT((#17325));
#17327=COLOUR_RGB('Black',0.12,0.14,0.17);
#17328=FILL_AREA_STYLE_COLOUR('',#17327);
#17329=FILL_AREA_STYLE('',(#17328));
#17330=SURFACE_STYLE_FILL_AREA(#17329);
#17331=SURFACE_SIDE_STYLE('',(#17330));
#17332=SURFACE_STYLE_USAGE(.BOTH.,#17331);
#17333=PRESENTATION_STYLE_ASSIGNMENT((#17332));
#17334=COLOUR_RGB('Off White',0.89,0.88,0.83);
#17335=FILL_AREA_STYLE_COLOUR('',#17334);
#17336=FILL_AREA_STYLE('',(#17335));
#17337=SURFACE_STYLE_FILL_AREA(#17336);
#17338=SURFACE_SIDE_STYLE('',(#17337));
#17339=SURFACE_STYLE_USAGE(.BOTH.,#17338);
#17340=PRESENTATION_STYLE_ASSIGNMENT((#17339));
ENDSEC;
END-ISO-10303-21;
